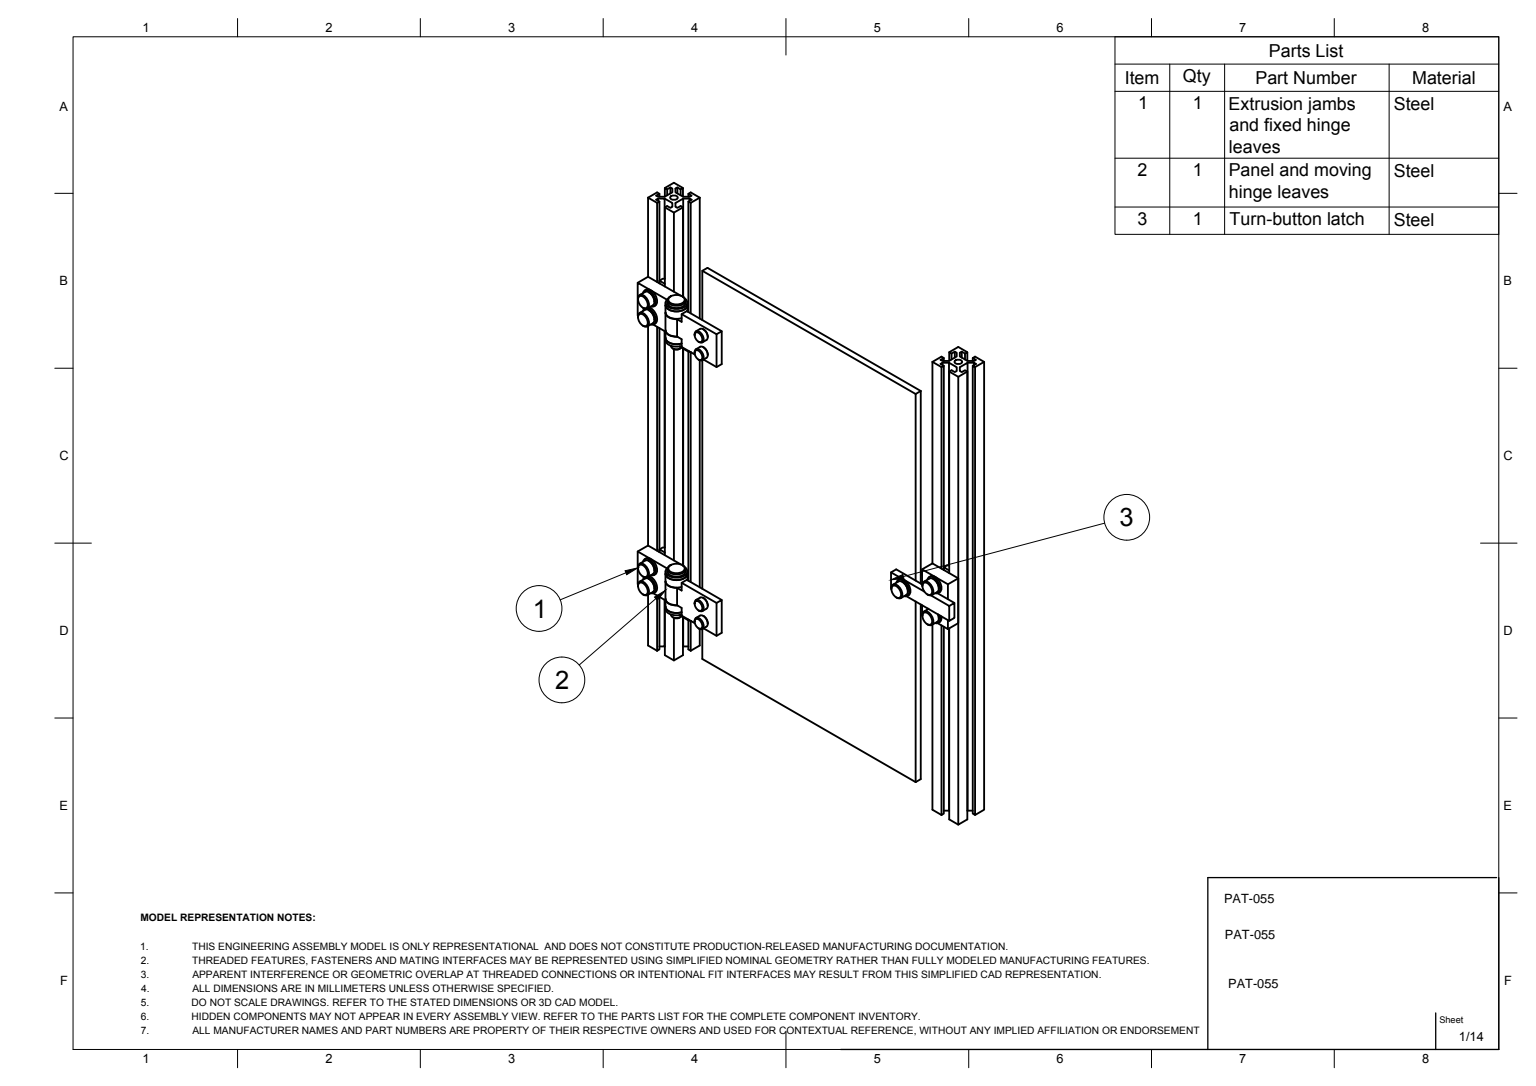
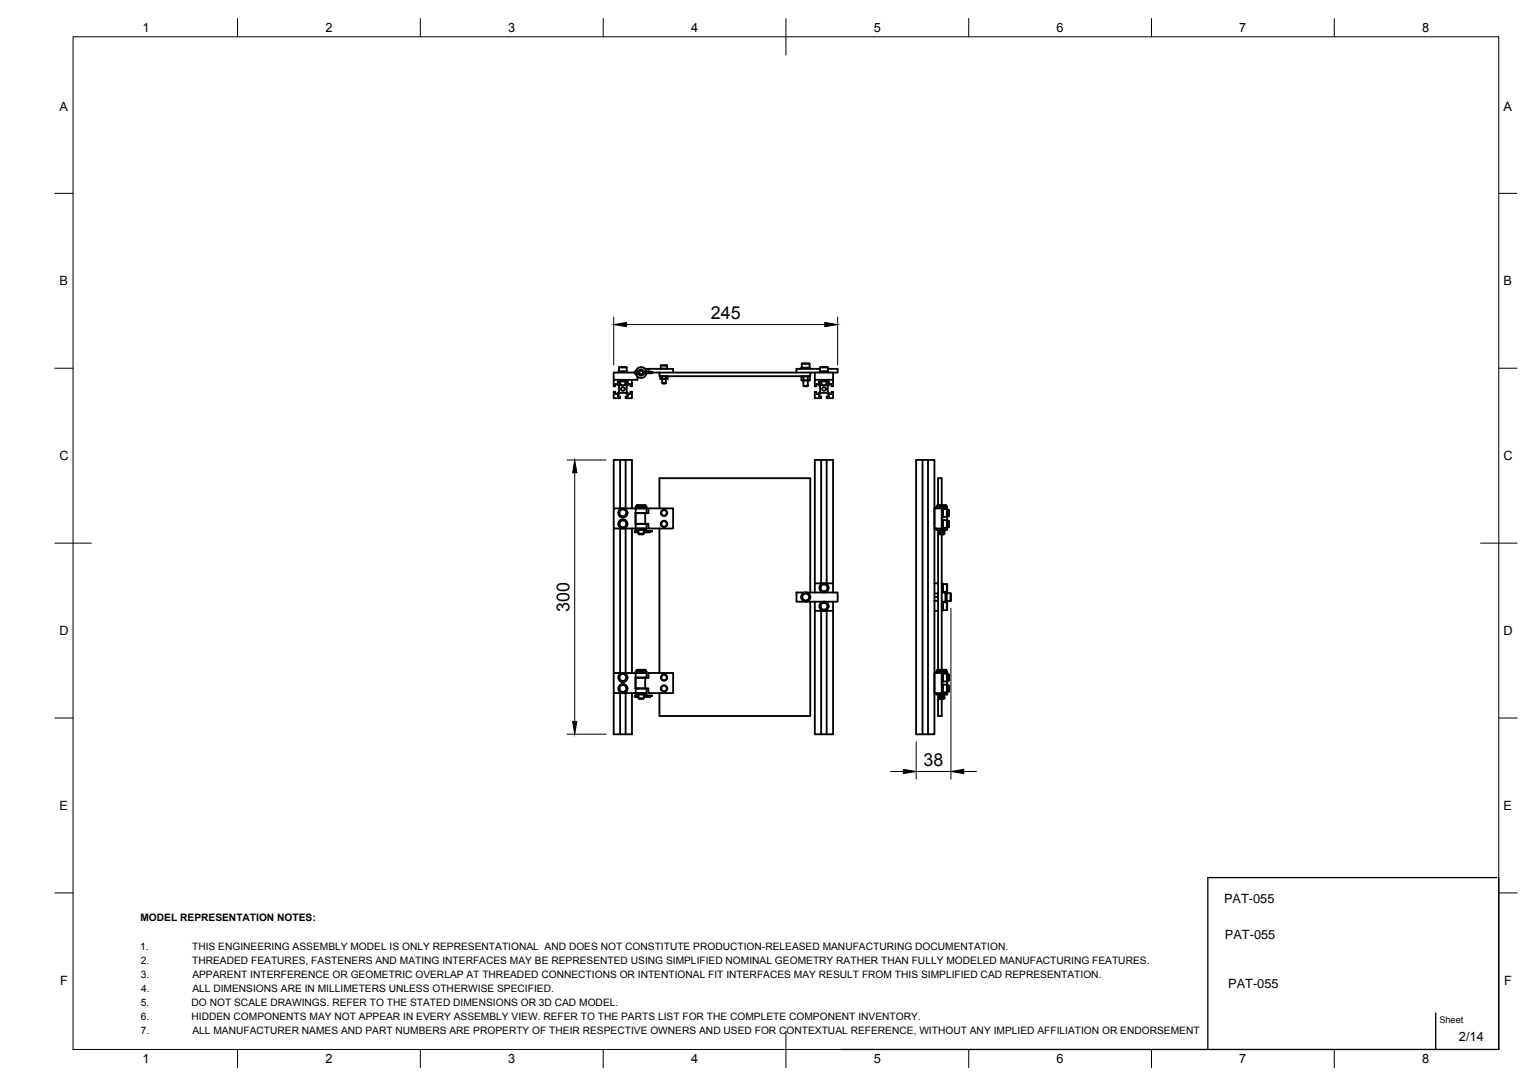
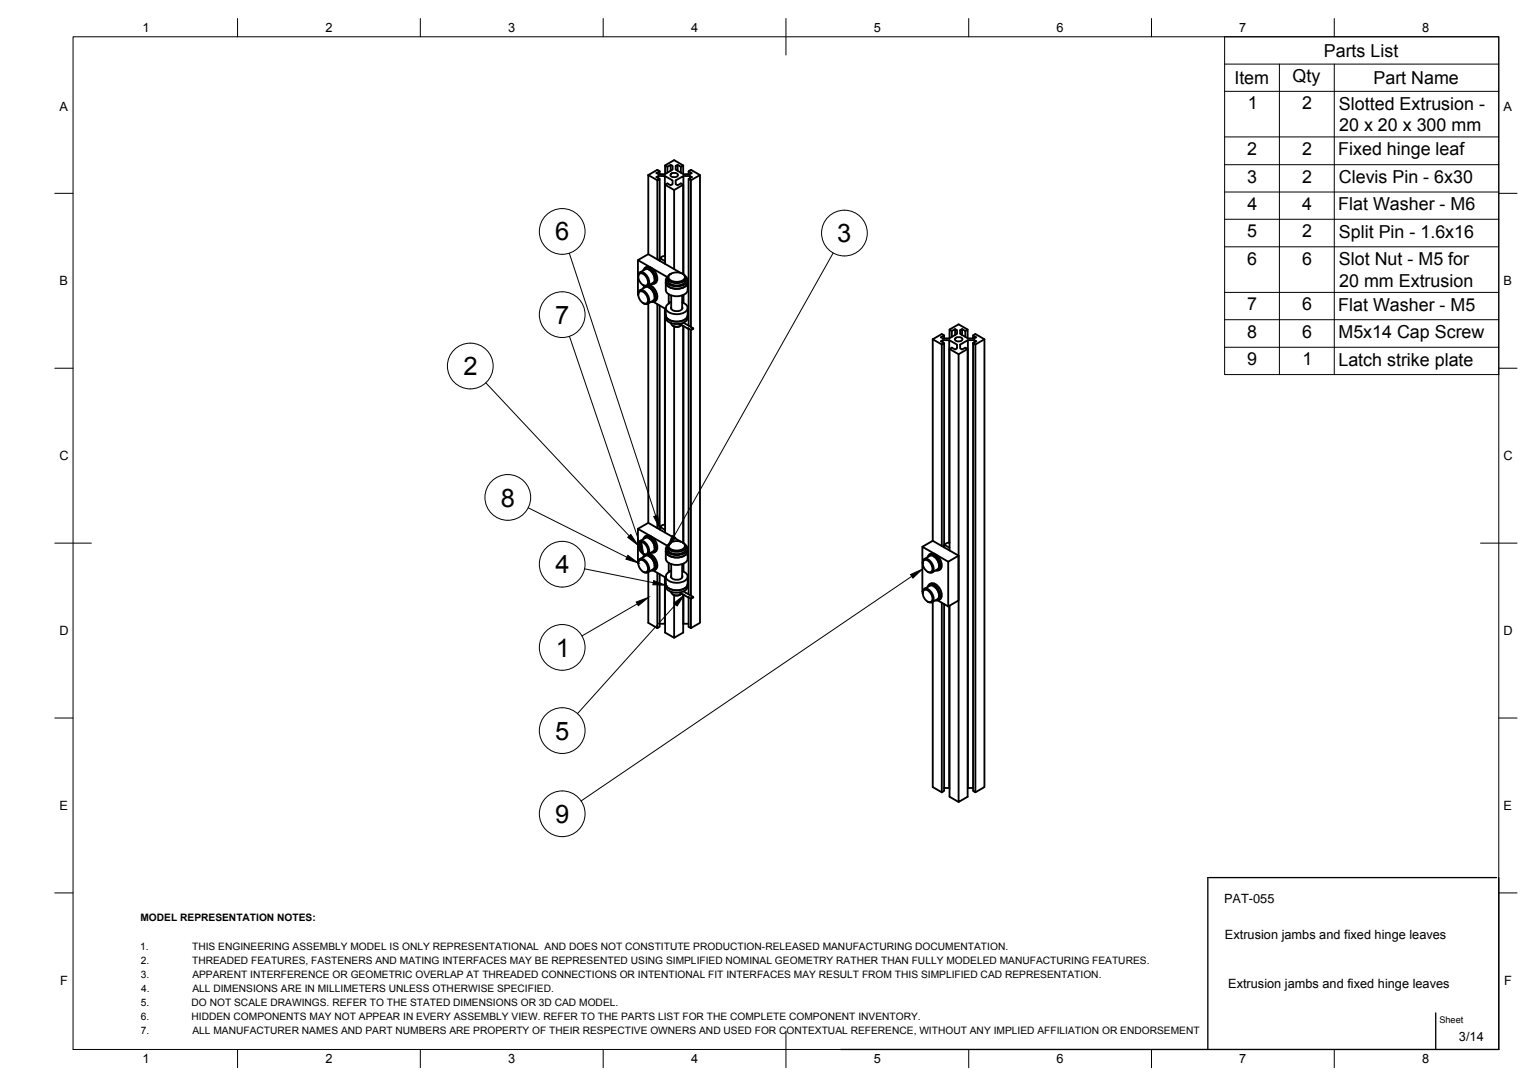
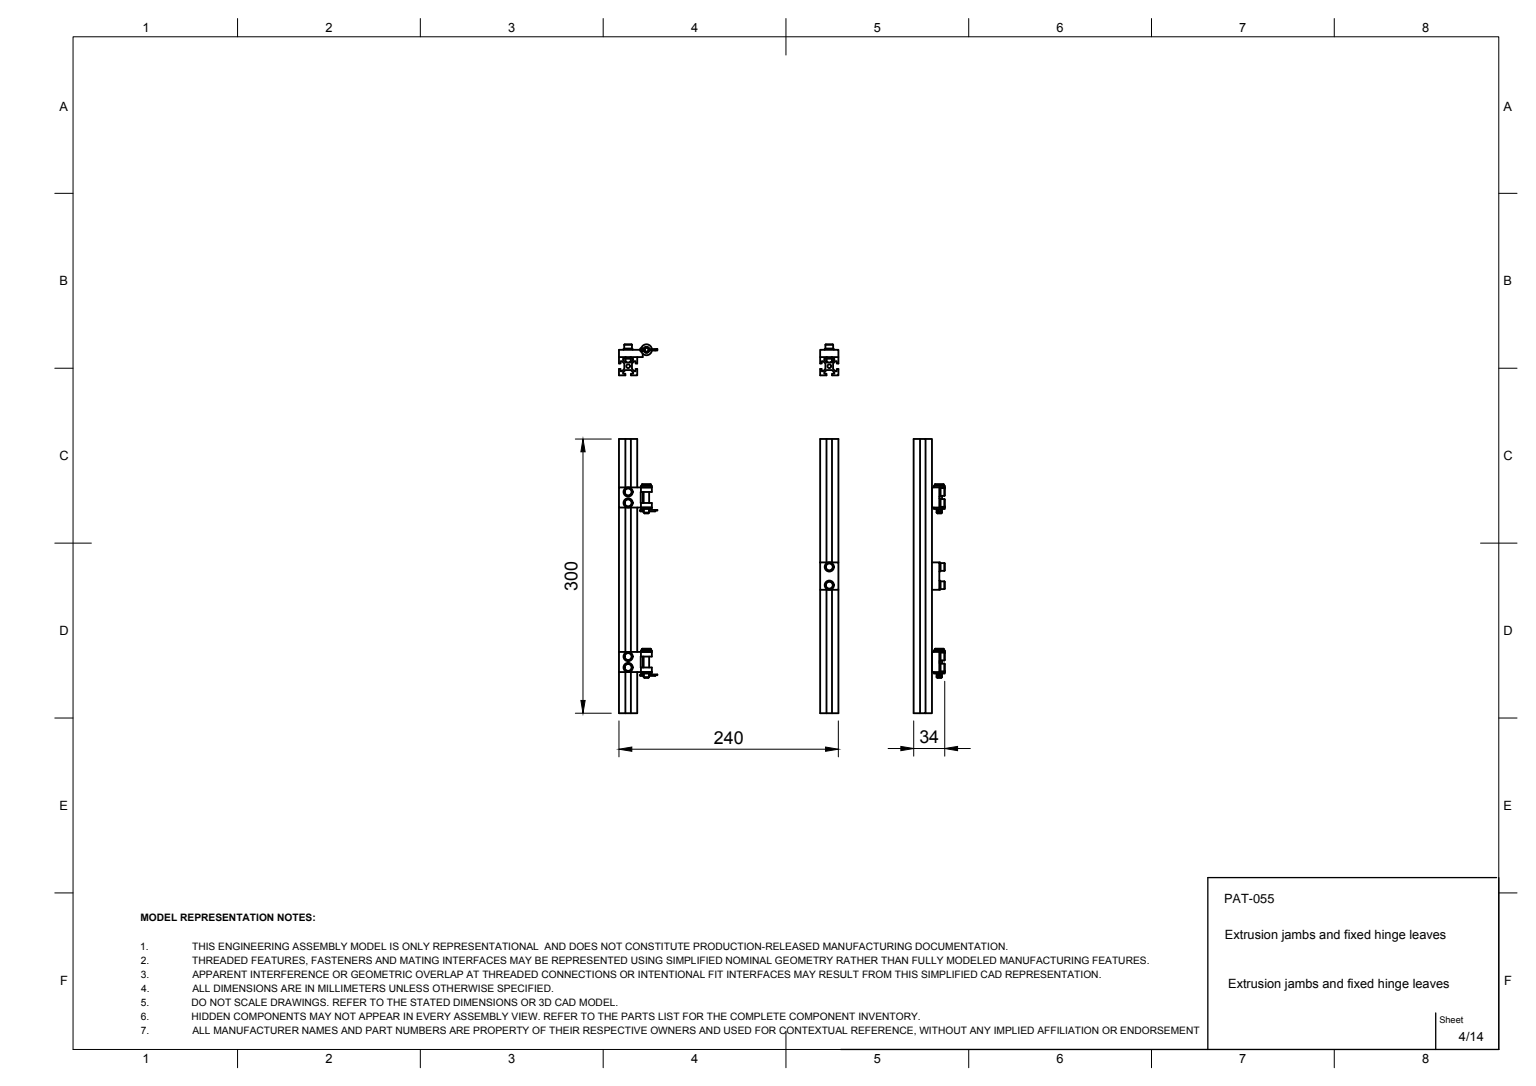
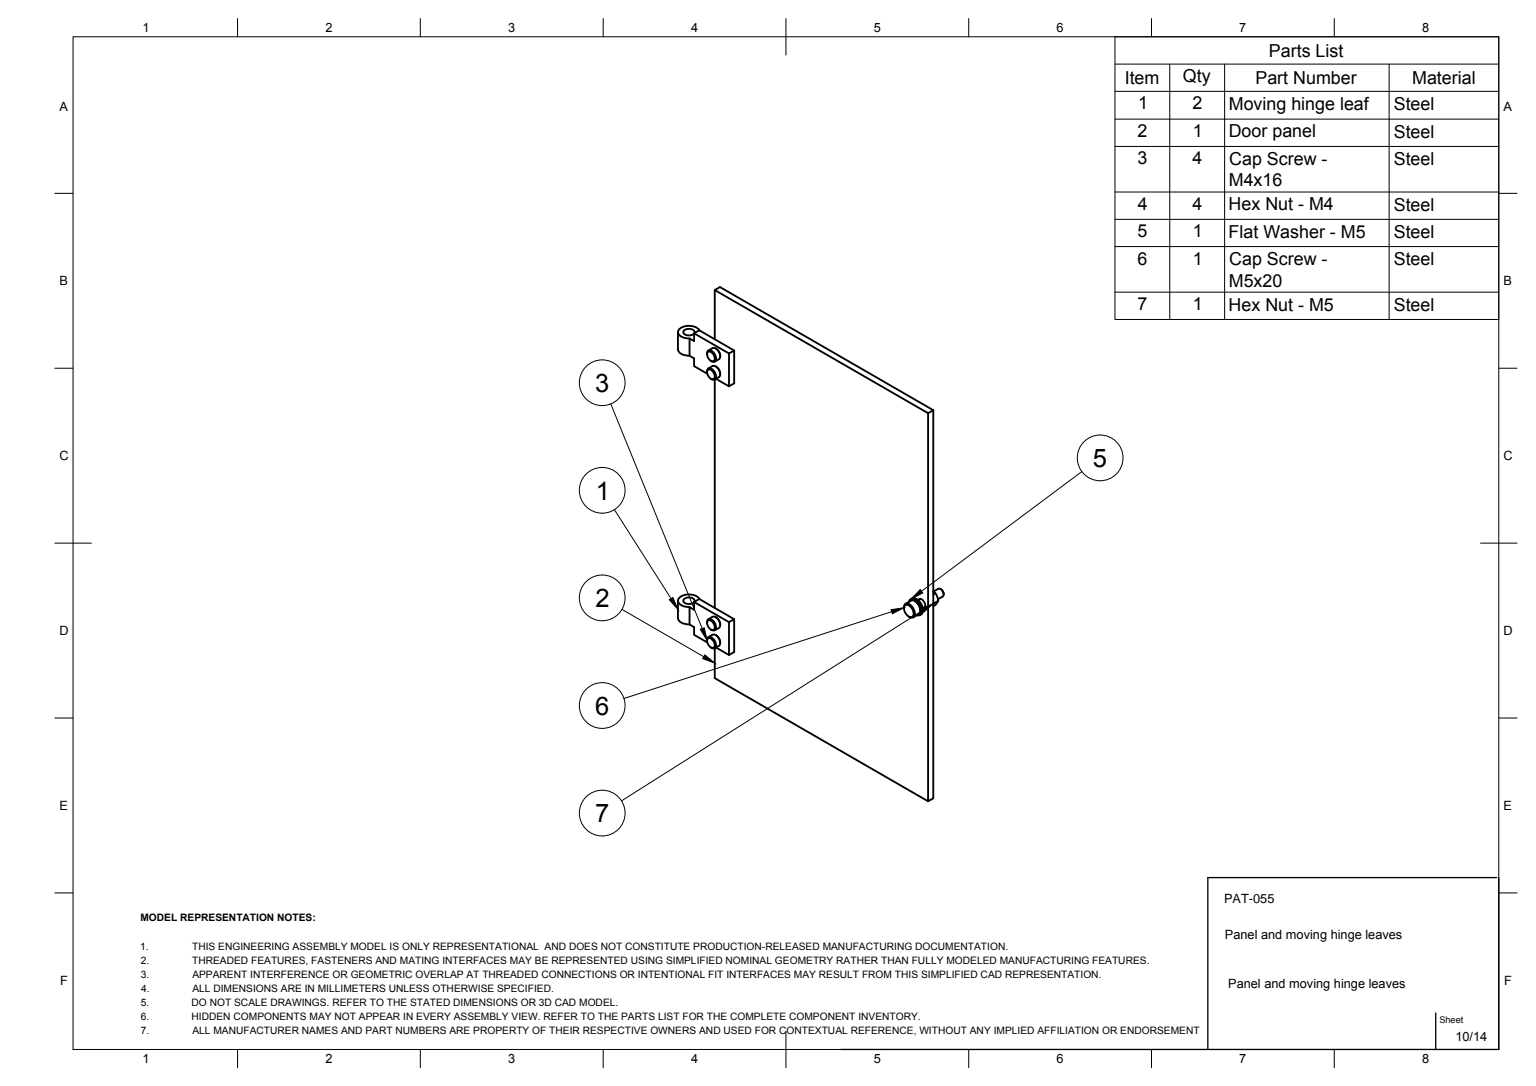
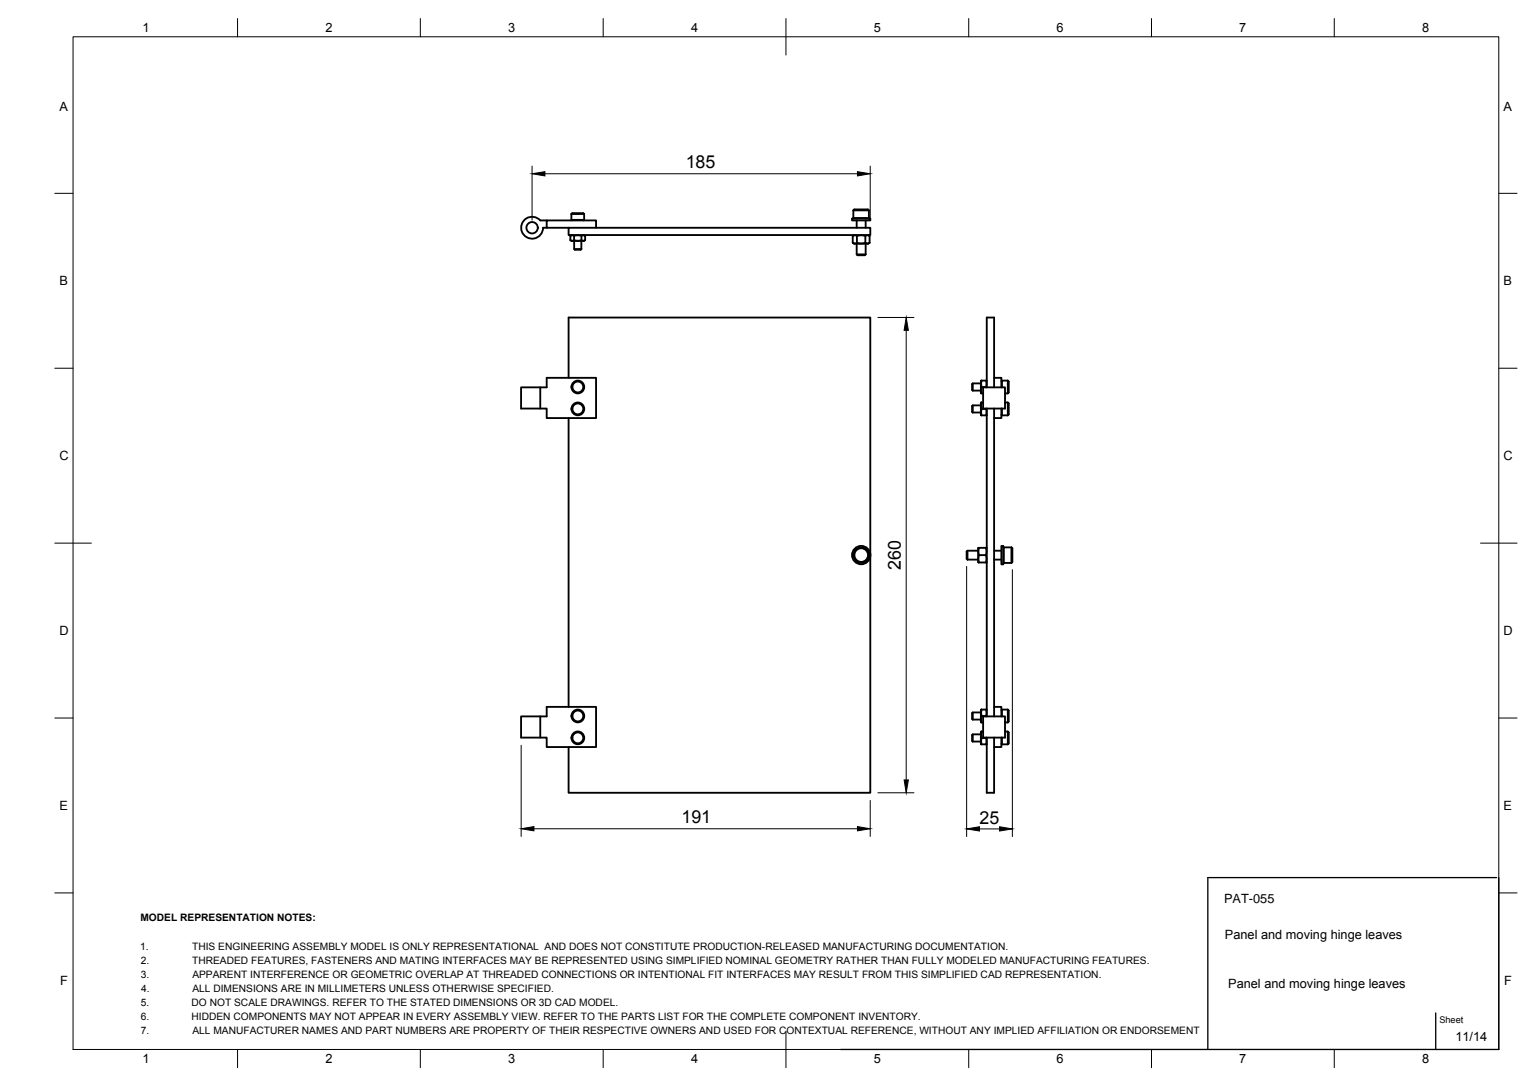
ISO-10303-21;
HEADER;
/* Generated by software containing ST-Developer
 * from STEP Tools, Inc. (www.steptools.com) 
 */

FILE_DESCRIPTION(
/* description */ ('Hinged panel with latch'),
/* implementation_level */ '2;1');

FILE_NAME(
/* name */ 'PAT-055',
/* time_stamp */ '2026-10-27T20:36:01-07:00',
/* author */ (''),
/* organization */ (''),
/* preprocessor_version */ 'ST-DEVELOPER v20.2',
/* originating_system */ 'Autodesk Translation Framework v15.17.0.0',
/* authorisation */ '');

FILE_SCHEMA (('AUTOMOTIVE_DESIGN { 1 0 10303 214 3 1 1 }'));
ENDSEC;

DATA;
#10=MECHANICAL_DESIGN_GEOMETRIC_PRESENTATION_REPRESENTATION('',(#296,#297,
#298,#299,#300,#301,#302,#303,#304,#305,#306,#307,#308,#309,#310,#311),
#6743);
#11=ITEM_DEFINED_TRANSFORMATION($,$,#4059,#4262);
#12=ITEM_DEFINED_TRANSFORMATION($,$,#3996,#4263);
#13=ITEM_DEFINED_TRANSFORMATION($,$,#4009,#4264);
#14=ITEM_DEFINED_TRANSFORMATION($,$,#4009,#4265);
#15=ITEM_DEFINED_TRANSFORMATION($,$,#4059,#4266);
#16=ITEM_DEFINED_TRANSFORMATION($,$,#4088,#4267);
#17=ITEM_DEFINED_TRANSFORMATION($,$,#4103,#4268);
#18=ITEM_DEFINED_TRANSFORMATION($,$,#4103,#4269);
#19=ITEM_DEFINED_TRANSFORMATION($,$,#4112,#4270);
#20=ITEM_DEFINED_TRANSFORMATION($,$,#4123,#4271);
#21=ITEM_DEFINED_TRANSFORMATION($,$,#4251,#4272);
#22=ITEM_DEFINED_TRANSFORMATION($,$,#4140,#4273);
#23=ITEM_DEFINED_TRANSFORMATION($,$,#4123,#4274);
#24=ITEM_DEFINED_TRANSFORMATION($,$,#4251,#4275);
#25=ITEM_DEFINED_TRANSFORMATION($,$,#4140,#4276);
#26=ITEM_DEFINED_TRANSFORMATION($,$,#4088,#4277);
#27=ITEM_DEFINED_TRANSFORMATION($,$,#4103,#4278);
#28=ITEM_DEFINED_TRANSFORMATION($,$,#4103,#4279);
#29=ITEM_DEFINED_TRANSFORMATION($,$,#4112,#4280);
#30=ITEM_DEFINED_TRANSFORMATION($,$,#4123,#4281);
#31=ITEM_DEFINED_TRANSFORMATION($,$,#4251,#4282);
#32=ITEM_DEFINED_TRANSFORMATION($,$,#4140,#4283);
#33=ITEM_DEFINED_TRANSFORMATION($,$,#4123,#4284);
#34=ITEM_DEFINED_TRANSFORMATION($,$,#4251,#4285);
#35=ITEM_DEFINED_TRANSFORMATION($,$,#4140,#4286);
#36=ITEM_DEFINED_TRANSFORMATION($,$,#4123,#4287);
#37=ITEM_DEFINED_TRANSFORMATION($,$,#4251,#4288);
#38=ITEM_DEFINED_TRANSFORMATION($,$,#4140,#4289);
#39=ITEM_DEFINED_TRANSFORMATION($,$,#4123,#4290);
#40=ITEM_DEFINED_TRANSFORMATION($,$,#4251,#4291);
#41=ITEM_DEFINED_TRANSFORMATION($,$,#4140,#4292);
#42=ITEM_DEFINED_TRANSFORMATION($,$,#4187,#4335);
#43=ITEM_DEFINED_TRANSFORMATION($,$,#4165,#4336);
#44=ITEM_DEFINED_TRANSFORMATION($,$,#4187,#4337);
#45=ITEM_DEFINED_TRANSFORMATION($,$,#4209,#4338);
#46=ITEM_DEFINED_TRANSFORMATION($,$,#4235,#4339);
#47=ITEM_DEFINED_TRANSFORMATION($,$,#4209,#4340);
#48=ITEM_DEFINED_TRANSFORMATION($,$,#4235,#4341);
#49=ITEM_DEFINED_TRANSFORMATION($,$,#4209,#4342);
#50=ITEM_DEFINED_TRANSFORMATION($,$,#4235,#4343);
#51=ITEM_DEFINED_TRANSFORMATION($,$,#4209,#4344);
#52=ITEM_DEFINED_TRANSFORMATION($,$,#4235,#4345);
#53=ITEM_DEFINED_TRANSFORMATION($,$,#4251,#4346);
#54=ITEM_DEFINED_TRANSFORMATION($,$,#4293,#4347);
#55=ITEM_DEFINED_TRANSFORMATION($,$,#4319,#4348);
#56=ITEM_DEFINED_TRANSFORMATION($,$,#4350,#4360);
#57=ITEM_DEFINED_TRANSFORMATION($,$,#3995,#4361);
#58=ITEM_DEFINED_TRANSFORMATION($,$,#4164,#4362);
#59=ITEM_DEFINED_TRANSFORMATION($,$,#4349,#4363);
#60=(
REPRESENTATION_RELATIONSHIP($,$,#6841,#6838)
REPRESENTATION_RELATIONSHIP_WITH_TRANSFORMATION(#11)
SHAPE_REPRESENTATION_RELATIONSHIP()
);
#61=(
REPRESENTATION_RELATIONSHIP($,$,#6839,#6838)
REPRESENTATION_RELATIONSHIP_WITH_TRANSFORMATION(#12)
SHAPE_REPRESENTATION_RELATIONSHIP()
);
#62=(
REPRESENTATION_RELATIONSHIP($,$,#6840,#6838)
REPRESENTATION_RELATIONSHIP_WITH_TRANSFORMATION(#13)
SHAPE_REPRESENTATION_RELATIONSHIP()
);
#63=(
REPRESENTATION_RELATIONSHIP($,$,#6840,#6838)
REPRESENTATION_RELATIONSHIP_WITH_TRANSFORMATION(#14)
SHAPE_REPRESENTATION_RELATIONSHIP()
);
#64=(
REPRESENTATION_RELATIONSHIP($,$,#6841,#6838)
REPRESENTATION_RELATIONSHIP_WITH_TRANSFORMATION(#15)
SHAPE_REPRESENTATION_RELATIONSHIP()
);
#65=(
REPRESENTATION_RELATIONSHIP($,$,#6842,#6838)
REPRESENTATION_RELATIONSHIP_WITH_TRANSFORMATION(#16)
SHAPE_REPRESENTATION_RELATIONSHIP()
);
#66=(
REPRESENTATION_RELATIONSHIP($,$,#6843,#6838)
REPRESENTATION_RELATIONSHIP_WITH_TRANSFORMATION(#17)
SHAPE_REPRESENTATION_RELATIONSHIP()
);
#67=(
REPRESENTATION_RELATIONSHIP($,$,#6843,#6838)
REPRESENTATION_RELATIONSHIP_WITH_TRANSFORMATION(#18)
SHAPE_REPRESENTATION_RELATIONSHIP()
);
#68=(
REPRESENTATION_RELATIONSHIP($,$,#6844,#6838)
REPRESENTATION_RELATIONSHIP_WITH_TRANSFORMATION(#19)
SHAPE_REPRESENTATION_RELATIONSHIP()
);
#69=(
REPRESENTATION_RELATIONSHIP($,$,#6845,#6838)
REPRESENTATION_RELATIONSHIP_WITH_TRANSFORMATION(#20)
SHAPE_REPRESENTATION_RELATIONSHIP()
);
#70=(
REPRESENTATION_RELATIONSHIP($,$,#6852,#6838)
REPRESENTATION_RELATIONSHIP_WITH_TRANSFORMATION(#21)
SHAPE_REPRESENTATION_RELATIONSHIP()
);
#71=(
REPRESENTATION_RELATIONSHIP($,$,#6846,#6838)
REPRESENTATION_RELATIONSHIP_WITH_TRANSFORMATION(#22)
SHAPE_REPRESENTATION_RELATIONSHIP()
);
#72=(
REPRESENTATION_RELATIONSHIP($,$,#6845,#6838)
REPRESENTATION_RELATIONSHIP_WITH_TRANSFORMATION(#23)
SHAPE_REPRESENTATION_RELATIONSHIP()
);
#73=(
REPRESENTATION_RELATIONSHIP($,$,#6852,#6838)
REPRESENTATION_RELATIONSHIP_WITH_TRANSFORMATION(#24)
SHAPE_REPRESENTATION_RELATIONSHIP()
);
#74=(
REPRESENTATION_RELATIONSHIP($,$,#6846,#6838)
REPRESENTATION_RELATIONSHIP_WITH_TRANSFORMATION(#25)
SHAPE_REPRESENTATION_RELATIONSHIP()
);
#75=(
REPRESENTATION_RELATIONSHIP($,$,#6842,#6838)
REPRESENTATION_RELATIONSHIP_WITH_TRANSFORMATION(#26)
SHAPE_REPRESENTATION_RELATIONSHIP()
);
#76=(
REPRESENTATION_RELATIONSHIP($,$,#6843,#6838)
REPRESENTATION_RELATIONSHIP_WITH_TRANSFORMATION(#27)
SHAPE_REPRESENTATION_RELATIONSHIP()
);
#77=(
REPRESENTATION_RELATIONSHIP($,$,#6843,#6838)
REPRESENTATION_RELATIONSHIP_WITH_TRANSFORMATION(#28)
SHAPE_REPRESENTATION_RELATIONSHIP()
);
#78=(
REPRESENTATION_RELATIONSHIP($,$,#6844,#6838)
REPRESENTATION_RELATIONSHIP_WITH_TRANSFORMATION(#29)
SHAPE_REPRESENTATION_RELATIONSHIP()
);
#79=(
REPRESENTATION_RELATIONSHIP($,$,#6845,#6838)
REPRESENTATION_RELATIONSHIP_WITH_TRANSFORMATION(#30)
SHAPE_REPRESENTATION_RELATIONSHIP()
);
#80=(
REPRESENTATION_RELATIONSHIP($,$,#6852,#6838)
REPRESENTATION_RELATIONSHIP_WITH_TRANSFORMATION(#31)
SHAPE_REPRESENTATION_RELATIONSHIP()
);
#81=(
REPRESENTATION_RELATIONSHIP($,$,#6846,#6838)
REPRESENTATION_RELATIONSHIP_WITH_TRANSFORMATION(#32)
SHAPE_REPRESENTATION_RELATIONSHIP()
);
#82=(
REPRESENTATION_RELATIONSHIP($,$,#6845,#6838)
REPRESENTATION_RELATIONSHIP_WITH_TRANSFORMATION(#33)
SHAPE_REPRESENTATION_RELATIONSHIP()
);
#83=(
REPRESENTATION_RELATIONSHIP($,$,#6852,#6838)
REPRESENTATION_RELATIONSHIP_WITH_TRANSFORMATION(#34)
SHAPE_REPRESENTATION_RELATIONSHIP()
);
#84=(
REPRESENTATION_RELATIONSHIP($,$,#6846,#6838)
REPRESENTATION_RELATIONSHIP_WITH_TRANSFORMATION(#35)
SHAPE_REPRESENTATION_RELATIONSHIP()
);
#85=(
REPRESENTATION_RELATIONSHIP($,$,#6845,#6838)
REPRESENTATION_RELATIONSHIP_WITH_TRANSFORMATION(#36)
SHAPE_REPRESENTATION_RELATIONSHIP()
);
#86=(
REPRESENTATION_RELATIONSHIP($,$,#6852,#6838)
REPRESENTATION_RELATIONSHIP_WITH_TRANSFORMATION(#37)
SHAPE_REPRESENTATION_RELATIONSHIP()
);
#87=(
REPRESENTATION_RELATIONSHIP($,$,#6846,#6838)
REPRESENTATION_RELATIONSHIP_WITH_TRANSFORMATION(#38)
SHAPE_REPRESENTATION_RELATIONSHIP()
);
#88=(
REPRESENTATION_RELATIONSHIP($,$,#6845,#6838)
REPRESENTATION_RELATIONSHIP_WITH_TRANSFORMATION(#39)
SHAPE_REPRESENTATION_RELATIONSHIP()
);
#89=(
REPRESENTATION_RELATIONSHIP($,$,#6852,#6838)
REPRESENTATION_RELATIONSHIP_WITH_TRANSFORMATION(#40)
SHAPE_REPRESENTATION_RELATIONSHIP()
);
#90=(
REPRESENTATION_RELATIONSHIP($,$,#6846,#6838)
REPRESENTATION_RELATIONSHIP_WITH_TRANSFORMATION(#41)
SHAPE_REPRESENTATION_RELATIONSHIP()
);
#91=(
REPRESENTATION_RELATIONSHIP($,$,#6849,#6847)
REPRESENTATION_RELATIONSHIP_WITH_TRANSFORMATION(#42)
SHAPE_REPRESENTATION_RELATIONSHIP()
);
#92=(
REPRESENTATION_RELATIONSHIP($,$,#6848,#6847)
REPRESENTATION_RELATIONSHIP_WITH_TRANSFORMATION(#43)
SHAPE_REPRESENTATION_RELATIONSHIP()
);
#93=(
REPRESENTATION_RELATIONSHIP($,$,#6849,#6847)
REPRESENTATION_RELATIONSHIP_WITH_TRANSFORMATION(#44)
SHAPE_REPRESENTATION_RELATIONSHIP()
);
#94=(
REPRESENTATION_RELATIONSHIP($,$,#6850,#6847)
REPRESENTATION_RELATIONSHIP_WITH_TRANSFORMATION(#45)
SHAPE_REPRESENTATION_RELATIONSHIP()
);
#95=(
REPRESENTATION_RELATIONSHIP($,$,#6851,#6847)
REPRESENTATION_RELATIONSHIP_WITH_TRANSFORMATION(#46)
SHAPE_REPRESENTATION_RELATIONSHIP()
);
#96=(
REPRESENTATION_RELATIONSHIP($,$,#6850,#6847)
REPRESENTATION_RELATIONSHIP_WITH_TRANSFORMATION(#47)
SHAPE_REPRESENTATION_RELATIONSHIP()
);
#97=(
REPRESENTATION_RELATIONSHIP($,$,#6851,#6847)
REPRESENTATION_RELATIONSHIP_WITH_TRANSFORMATION(#48)
SHAPE_REPRESENTATION_RELATIONSHIP()
);
#98=(
REPRESENTATION_RELATIONSHIP($,$,#6850,#6847)
REPRESENTATION_RELATIONSHIP_WITH_TRANSFORMATION(#49)
SHAPE_REPRESENTATION_RELATIONSHIP()
);
#99=(
REPRESENTATION_RELATIONSHIP($,$,#6851,#6847)
REPRESENTATION_RELATIONSHIP_WITH_TRANSFORMATION(#50)
SHAPE_REPRESENTATION_RELATIONSHIP()
);
#100=(
REPRESENTATION_RELATIONSHIP($,$,#6850,#6847)
REPRESENTATION_RELATIONSHIP_WITH_TRANSFORMATION(#51)
SHAPE_REPRESENTATION_RELATIONSHIP()
);
#101=(
REPRESENTATION_RELATIONSHIP($,$,#6851,#6847)
REPRESENTATION_RELATIONSHIP_WITH_TRANSFORMATION(#52)
SHAPE_REPRESENTATION_RELATIONSHIP()
);
#102=(
REPRESENTATION_RELATIONSHIP($,$,#6852,#6847)
REPRESENTATION_RELATIONSHIP_WITH_TRANSFORMATION(#53)
SHAPE_REPRESENTATION_RELATIONSHIP()
);
#103=(
REPRESENTATION_RELATIONSHIP($,$,#6853,#6847)
REPRESENTATION_RELATIONSHIP_WITH_TRANSFORMATION(#54)
SHAPE_REPRESENTATION_RELATIONSHIP()
);
#104=(
REPRESENTATION_RELATIONSHIP($,$,#6854,#6847)
REPRESENTATION_RELATIONSHIP_WITH_TRANSFORMATION(#55)
SHAPE_REPRESENTATION_RELATIONSHIP()
);
#105=(
REPRESENTATION_RELATIONSHIP($,$,#6856,#6855)
REPRESENTATION_RELATIONSHIP_WITH_TRANSFORMATION(#56)
SHAPE_REPRESENTATION_RELATIONSHIP()
);
#106=(
REPRESENTATION_RELATIONSHIP($,$,#6838,#6837)
REPRESENTATION_RELATIONSHIP_WITH_TRANSFORMATION(#57)
SHAPE_REPRESENTATION_RELATIONSHIP()
);
#107=(
REPRESENTATION_RELATIONSHIP($,$,#6847,#6837)
REPRESENTATION_RELATIONSHIP_WITH_TRANSFORMATION(#58)
SHAPE_REPRESENTATION_RELATIONSHIP()
);
#108=(
REPRESENTATION_RELATIONSHIP($,$,#6855,#6837)
REPRESENTATION_RELATIONSHIP_WITH_TRANSFORMATION(#59)
SHAPE_REPRESENTATION_RELATIONSHIP()
);
#109=CONTEXT_DEPENDENT_SHAPE_REPRESENTATION(#60,#6784);
#110=CONTEXT_DEPENDENT_SHAPE_REPRESENTATION(#61,#6785);
#111=CONTEXT_DEPENDENT_SHAPE_REPRESENTATION(#62,#6786);
#112=CONTEXT_DEPENDENT_SHAPE_REPRESENTATION(#63,#6787);
#113=CONTEXT_DEPENDENT_SHAPE_REPRESENTATION(#64,#6788);
#114=CONTEXT_DEPENDENT_SHAPE_REPRESENTATION(#65,#6789);
#115=CONTEXT_DEPENDENT_SHAPE_REPRESENTATION(#66,#6790);
#116=CONTEXT_DEPENDENT_SHAPE_REPRESENTATION(#67,#6791);
#117=CONTEXT_DEPENDENT_SHAPE_REPRESENTATION(#68,#6792);
#118=CONTEXT_DEPENDENT_SHAPE_REPRESENTATION(#69,#6793);
#119=CONTEXT_DEPENDENT_SHAPE_REPRESENTATION(#70,#6794);
#120=CONTEXT_DEPENDENT_SHAPE_REPRESENTATION(#71,#6795);
#121=CONTEXT_DEPENDENT_SHAPE_REPRESENTATION(#72,#6796);
#122=CONTEXT_DEPENDENT_SHAPE_REPRESENTATION(#73,#6797);
#123=CONTEXT_DEPENDENT_SHAPE_REPRESENTATION(#74,#6798);
#124=CONTEXT_DEPENDENT_SHAPE_REPRESENTATION(#75,#6799);
#125=CONTEXT_DEPENDENT_SHAPE_REPRESENTATION(#76,#6800);
#126=CONTEXT_DEPENDENT_SHAPE_REPRESENTATION(#77,#6801);
#127=CONTEXT_DEPENDENT_SHAPE_REPRESENTATION(#78,#6802);
#128=CONTEXT_DEPENDENT_SHAPE_REPRESENTATION(#79,#6803);
#129=CONTEXT_DEPENDENT_SHAPE_REPRESENTATION(#80,#6804);
#130=CONTEXT_DEPENDENT_SHAPE_REPRESENTATION(#81,#6805);
#131=CONTEXT_DEPENDENT_SHAPE_REPRESENTATION(#82,#6806);
#132=CONTEXT_DEPENDENT_SHAPE_REPRESENTATION(#83,#6807);
#133=CONTEXT_DEPENDENT_SHAPE_REPRESENTATION(#84,#6808);
#134=CONTEXT_DEPENDENT_SHAPE_REPRESENTATION(#85,#6809);
#135=CONTEXT_DEPENDENT_SHAPE_REPRESENTATION(#86,#6810);
#136=CONTEXT_DEPENDENT_SHAPE_REPRESENTATION(#87,#6811);
#137=CONTEXT_DEPENDENT_SHAPE_REPRESENTATION(#88,#6812);
#138=CONTEXT_DEPENDENT_SHAPE_REPRESENTATION(#89,#6813);
#139=CONTEXT_DEPENDENT_SHAPE_REPRESENTATION(#90,#6814);
#140=CONTEXT_DEPENDENT_SHAPE_REPRESENTATION(#91,#6817);
#141=CONTEXT_DEPENDENT_SHAPE_REPRESENTATION(#92,#6818);
#142=CONTEXT_DEPENDENT_SHAPE_REPRESENTATION(#93,#6819);
#143=CONTEXT_DEPENDENT_SHAPE_REPRESENTATION(#94,#6820);
#144=CONTEXT_DEPENDENT_SHAPE_REPRESENTATION(#95,#6821);
#145=CONTEXT_DEPENDENT_SHAPE_REPRESENTATION(#96,#6822);
#146=CONTEXT_DEPENDENT_SHAPE_REPRESENTATION(#97,#6823);
#147=CONTEXT_DEPENDENT_SHAPE_REPRESENTATION(#98,#6824);
#148=CONTEXT_DEPENDENT_SHAPE_REPRESENTATION(#99,#6825);
#149=CONTEXT_DEPENDENT_SHAPE_REPRESENTATION(#100,#6826);
#150=CONTEXT_DEPENDENT_SHAPE_REPRESENTATION(#101,#6827);
#151=CONTEXT_DEPENDENT_SHAPE_REPRESENTATION(#102,#6828);
#152=CONTEXT_DEPENDENT_SHAPE_REPRESENTATION(#103,#6829);
#153=CONTEXT_DEPENDENT_SHAPE_REPRESENTATION(#104,#6830);
#154=CONTEXT_DEPENDENT_SHAPE_REPRESENTATION(#105,#6833);
#155=CONTEXT_DEPENDENT_SHAPE_REPRESENTATION(#106,#6834);
#156=CONTEXT_DEPENDENT_SHAPE_REPRESENTATION(#107,#6835);
#157=CONTEXT_DEPENDENT_SHAPE_REPRESENTATION(#108,#6836);
#158=NEXT_ASSEMBLY_USAGE_OCCURRENCE('Fixed hinge leaf:1',
'Fixed hinge leaf:1','Fixed hinge leaf:1',#6859,#6862,
'Fixed hinge leaf:1');
#159=NEXT_ASSEMBLY_USAGE_OCCURRENCE('Latch strike plate:1',
'Latch strike plate:1','Latch strike plate:1',#6859,#6860,
'Latch strike plate:1');
#160=NEXT_ASSEMBLY_USAGE_OCCURRENCE(
'Slotted Extrusion - 20 x 20 x 300 mm:2',
'Slotted Extrusion - 20 x 20 x 300 mm:2',
'Slotted Extrusion - 20 x 20 x 300 mm:2',#6859,#6861,
'Slotted Extrusion - 20 x 20 x 300 mm:2');
#161=NEXT_ASSEMBLY_USAGE_OCCURRENCE(
'Slotted Extrusion - 20 x 20 x 300 mm:3',
'Slotted Extrusion - 20 x 20 x 300 mm:3',
'Slotted Extrusion - 20 x 20 x 300 mm:3',#6859,#6861,
'Slotted Extrusion - 20 x 20 x 300 mm:3');
#162=NEXT_ASSEMBLY_USAGE_OCCURRENCE('Fixed hinge leaf:2',
'Fixed hinge leaf:2','Fixed hinge leaf:2',#6859,#6862,
'Fixed hinge leaf:2');
#163=NEXT_ASSEMBLY_USAGE_OCCURRENCE('Clevis Pin - 6x30:2',
'Clevis Pin - 6x30:2','Clevis Pin - 6x30:2',#6859,#6863,
'Clevis Pin - 6x30:2');
#164=NEXT_ASSEMBLY_USAGE_OCCURRENCE('Flat Washer - M6:2',
'Flat Washer - M6:2','Flat Washer - M6:2',#6859,#6864,
'Flat Washer - M6:2');
#165=NEXT_ASSEMBLY_USAGE_OCCURRENCE('Flat Washer - M6:3',
'Flat Washer - M6:3','Flat Washer - M6:3',#6859,#6864,
'Flat Washer - M6:3');
#166=NEXT_ASSEMBLY_USAGE_OCCURRENCE('Split Pin - 1.6x16:2',
'Split Pin - 1.6x16:2','Split Pin - 1.6x16:2',#6859,#6865,
'Split Pin - 1.6x16:2');
#167=NEXT_ASSEMBLY_USAGE_OCCURRENCE(
'Slot Nut - M5 for 20 mm Extrusion:2',
'Slot Nut - M5 for 20 mm Extrusion:2',
'Slot Nut - M5 for 20 mm Extrusion:2',#6859,#6866,
'Slot Nut - M5 for 20 mm Extrusion:2');
#168=NEXT_ASSEMBLY_USAGE_OCCURRENCE('Flat Washer - M5:2',
'Flat Washer - M5:2','Flat Washer - M5:2',#6859,#6873,
'Flat Washer - M5:2');
#169=NEXT_ASSEMBLY_USAGE_OCCURRENCE('M5x14 Cap Screw:2',
'M5x14 Cap Screw:2','M5x14 Cap Screw:2',#6859,#6867,'M5x14 Cap Screw:2');
#170=NEXT_ASSEMBLY_USAGE_OCCURRENCE(
'Slot Nut - M5 for 20 mm Extrusion:3',
'Slot Nut - M5 for 20 mm Extrusion:3',
'Slot Nut - M5 for 20 mm Extrusion:3',#6859,#6866,
'Slot Nut - M5 for 20 mm Extrusion:3');
#171=NEXT_ASSEMBLY_USAGE_OCCURRENCE('Flat Washer - M5:3',
'Flat Washer - M5:3','Flat Washer - M5:3',#6859,#6873,
'Flat Washer - M5:3');
#172=NEXT_ASSEMBLY_USAGE_OCCURRENCE('M5x14 Cap Screw:3',
'M5x14 Cap Screw:3','M5x14 Cap Screw:3',#6859,#6867,'M5x14 Cap Screw:3');
#173=NEXT_ASSEMBLY_USAGE_OCCURRENCE('Clevis Pin - 6x30:3',
'Clevis Pin - 6x30:3','Clevis Pin - 6x30:3',#6859,#6863,
'Clevis Pin - 6x30:3');
#174=NEXT_ASSEMBLY_USAGE_OCCURRENCE('Flat Washer - M6:4',
'Flat Washer - M6:4','Flat Washer - M6:4',#6859,#6864,
'Flat Washer - M6:4');
#175=NEXT_ASSEMBLY_USAGE_OCCURRENCE('Flat Washer - M6:5',
'Flat Washer - M6:5','Flat Washer - M6:5',#6859,#6864,
'Flat Washer - M6:5');
#176=NEXT_ASSEMBLY_USAGE_OCCURRENCE('Split Pin - 1.6x16:3',
'Split Pin - 1.6x16:3','Split Pin - 1.6x16:3',#6859,#6865,
'Split Pin - 1.6x16:3');
#177=NEXT_ASSEMBLY_USAGE_OCCURRENCE(
'Slot Nut - M5 for 20 mm Extrusion:4',
'Slot Nut - M5 for 20 mm Extrusion:4',
'Slot Nut - M5 for 20 mm Extrusion:4',#6859,#6866,
'Slot Nut - M5 for 20 mm Extrusion:4');
#178=NEXT_ASSEMBLY_USAGE_OCCURRENCE('Flat Washer - M5:4',
'Flat Washer - M5:4','Flat Washer - M5:4',#6859,#6873,
'Flat Washer - M5:4');
#179=NEXT_ASSEMBLY_USAGE_OCCURRENCE('M5x14 Cap Screw:4',
'M5x14 Cap Screw:4','M5x14 Cap Screw:4',#6859,#6867,'M5x14 Cap Screw:4');
#180=NEXT_ASSEMBLY_USAGE_OCCURRENCE(
'Slot Nut - M5 for 20 mm Extrusion:5',
'Slot Nut - M5 for 20 mm Extrusion:5',
'Slot Nut - M5 for 20 mm Extrusion:5',#6859,#6866,
'Slot Nut - M5 for 20 mm Extrusion:5');
#181=NEXT_ASSEMBLY_USAGE_OCCURRENCE('Flat Washer - M5:5',
'Flat Washer - M5:5','Flat Washer - M5:5',#6859,#6873,
'Flat Washer - M5:5');
#182=NEXT_ASSEMBLY_USAGE_OCCURRENCE('M5x14 Cap Screw:5',
'M5x14 Cap Screw:5','M5x14 Cap Screw:5',#6859,#6867,'M5x14 Cap Screw:5');
#183=NEXT_ASSEMBLY_USAGE_OCCURRENCE(
'Slot Nut - M5 for 20 mm Extrusion:6',
'Slot Nut - M5 for 20 mm Extrusion:6',
'Slot Nut - M5 for 20 mm Extrusion:6',#6859,#6866,
'Slot Nut - M5 for 20 mm Extrusion:6');
#184=NEXT_ASSEMBLY_USAGE_OCCURRENCE('Flat Washer - M5:6',
'Flat Washer - M5:6','Flat Washer - M5:6',#6859,#6873,
'Flat Washer - M5:6');
#185=NEXT_ASSEMBLY_USAGE_OCCURRENCE('M5x14 Cap Screw:6',
'M5x14 Cap Screw:6','M5x14 Cap Screw:6',#6859,#6867,'M5x14 Cap Screw:6');
#186=NEXT_ASSEMBLY_USAGE_OCCURRENCE(
'Slot Nut - M5 for 20 mm Extrusion:7',
'Slot Nut - M5 for 20 mm Extrusion:7',
'Slot Nut - M5 for 20 mm Extrusion:7',#6859,#6866,
'Slot Nut - M5 for 20 mm Extrusion:7');
#187=NEXT_ASSEMBLY_USAGE_OCCURRENCE('Flat Washer - M5:7',
'Flat Washer - M5:7','Flat Washer - M5:7',#6859,#6873,
'Flat Washer - M5:7');
#188=NEXT_ASSEMBLY_USAGE_OCCURRENCE('M5x14 Cap Screw:7',
'M5x14 Cap Screw:7','M5x14 Cap Screw:7',#6859,#6867,'M5x14 Cap Screw:7');
#189=NEXT_ASSEMBLY_USAGE_OCCURRENCE('Moving hinge leaf:1',
'Moving hinge leaf:1','Moving hinge leaf:1',#6868,#6870,
'Moving hinge leaf:1');
#190=NEXT_ASSEMBLY_USAGE_OCCURRENCE('Door panel:1','Door panel:1',
'Door panel:1',#6868,#6869,'Door panel:1');
#191=NEXT_ASSEMBLY_USAGE_OCCURRENCE('Moving hinge leaf:2',
'Moving hinge leaf:2','Moving hinge leaf:2',#6868,#6870,
'Moving hinge leaf:2');
#192=NEXT_ASSEMBLY_USAGE_OCCURRENCE('Cap Screw - M4x16:2',
'Cap Screw - M4x16:2','Cap Screw - M4x16:2',#6868,#6871,
'Cap Screw - M4x16:2');
#193=NEXT_ASSEMBLY_USAGE_OCCURRENCE('Hex Nut - M4:2','Hex Nut - M4:2',
'Hex Nut - M4:2',#6868,#6872,'Hex Nut - M4:2');
#194=NEXT_ASSEMBLY_USAGE_OCCURRENCE('Cap Screw - M4x16:3',
'Cap Screw - M4x16:3','Cap Screw - M4x16:3',#6868,#6871,
'Cap Screw - M4x16:3');
#195=NEXT_ASSEMBLY_USAGE_OCCURRENCE('Hex Nut - M4:3','Hex Nut - M4:3',
'Hex Nut - M4:3',#6868,#6872,'Hex Nut - M4:3');
#196=NEXT_ASSEMBLY_USAGE_OCCURRENCE('Cap Screw - M4x16:4',
'Cap Screw - M4x16:4','Cap Screw - M4x16:4',#6868,#6871,
'Cap Screw - M4x16:4');
#197=NEXT_ASSEMBLY_USAGE_OCCURRENCE('Hex Nut - M4:4','Hex Nut - M4:4',
'Hex Nut - M4:4',#6868,#6872,'Hex Nut - M4:4');
#198=NEXT_ASSEMBLY_USAGE_OCCURRENCE('Cap Screw - M4x16:5',
'Cap Screw - M4x16:5','Cap Screw - M4x16:5',#6868,#6871,
'Cap Screw - M4x16:5');
#199=NEXT_ASSEMBLY_USAGE_OCCURRENCE('Hex Nut - M4:5','Hex Nut - M4:5',
'Hex Nut - M4:5',#6868,#6872,'Hex Nut - M4:5');
#200=NEXT_ASSEMBLY_USAGE_OCCURRENCE('Flat Washer - M5:8',
'Flat Washer - M5:8','Flat Washer - M5:8',#6868,#6873,
'Flat Washer - M5:8');
#201=NEXT_ASSEMBLY_USAGE_OCCURRENCE('Cap Screw - M5x20:2',
'Cap Screw - M5x20:2','Cap Screw - M5x20:2',#6868,#6874,
'Cap Screw - M5x20:2');
#202=NEXT_ASSEMBLY_USAGE_OCCURRENCE('Hex Nut - M5:2','Hex Nut - M5:2',
'Hex Nut - M5:2',#6868,#6875,'Hex Nut - M5:2');
#203=NEXT_ASSEMBLY_USAGE_OCCURRENCE('Turn-button latch (1):1',
'Turn-button latch (1):1','Turn-button latch (1):1',#6876,#6877,
'Turn-button latch (1):1');
#204=NEXT_ASSEMBLY_USAGE_OCCURRENCE(
'Extrusion jambs and fixed hinge leaves:1',
'Extrusion jambs and fixed hinge leaves:1',
'Extrusion jambs and fixed hinge leaves:1',#6858,#6859,
'Extrusion jambs and fixed hinge leaves:1');
#205=NEXT_ASSEMBLY_USAGE_OCCURRENCE('Panel and moving hinge leaves:1',
'Panel and moving hinge leaves:1','Panel and moving hinge leaves:1',#6858,
#6868,'Panel and moving hinge leaves:1');
#206=NEXT_ASSEMBLY_USAGE_OCCURRENCE('Turn-button latch:1',
'Turn-button latch:1','Turn-button latch:1',#6858,#6876,
'Turn-button latch:1');
#207=(
BOUNDED_CURVE()
B_SPLINE_CURVE(2,(#6380,#6381,#6382),.UNSPECIFIED.,.F.,.F.)
B_SPLINE_CURVE_WITH_KNOTS((3,3),(0.137956735689167,0.609258407070138),
 .UNSPECIFIED.)
CURVE()
GEOMETRIC_REPRESENTATION_ITEM()
RATIONAL_B_SPLINE_CURVE((1.13260046146793,1.30781436262561,1.13260046146793))
REPRESENTATION_ITEM('')
);
#208=(
BOUNDED_CURVE()
B_SPLINE_CURVE(2,(#6384,#6385,#6386),.UNSPECIFIED.,.F.,.F.)
B_SPLINE_CURVE_WITH_KNOTS((3,3),(0.137956735689167,0.609258407070137),
 .UNSPECIFIED.)
CURVE()
GEOMETRIC_REPRESENTATION_ITEM()
RATIONAL_B_SPLINE_CURVE((1.13260046146793,1.30781436262561,1.13260046146793))
REPRESENTATION_ITEM('')
);
#209=(
BOUNDED_CURVE()
B_SPLINE_CURVE(2,(#6391,#6392,#6393),.UNSPECIFIED.,.F.,.F.)
B_SPLINE_CURVE_WITH_KNOTS((3,3),(0.137956735689167,0.609258407070138),
 .UNSPECIFIED.)
CURVE()
GEOMETRIC_REPRESENTATION_ITEM()
RATIONAL_B_SPLINE_CURVE((1.13260046146793,1.30781436262561,1.13260046146793))
REPRESENTATION_ITEM('')
);
#210=(
BOUNDED_CURVE()
B_SPLINE_CURVE(2,(#6395,#6396,#6397),.UNSPECIFIED.,.F.,.F.)
B_SPLINE_CURVE_WITH_KNOTS((3,3),(0.137956735689167,0.609258407070138),
 .UNSPECIFIED.)
CURVE()
GEOMETRIC_REPRESENTATION_ITEM()
RATIONAL_B_SPLINE_CURVE((1.13260046146793,1.30781436262561,1.13260046146793))
REPRESENTATION_ITEM('')
);
#211=(
BOUNDED_CURVE()
B_SPLINE_CURVE(2,(#6399,#6400,#6401),.UNSPECIFIED.,.F.,.F.)
B_SPLINE_CURVE_WITH_KNOTS((3,3),(0.137956735689167,0.609258407070138),
 .UNSPECIFIED.)
CURVE()
GEOMETRIC_REPRESENTATION_ITEM()
RATIONAL_B_SPLINE_CURVE((1.13260046146793,1.30781436262561,1.13260046146793))
REPRESENTATION_ITEM('')
);
#212=(
BOUNDED_CURVE()
B_SPLINE_CURVE(2,(#6402,#6403,#6404),.UNSPECIFIED.,.F.,.F.)
B_SPLINE_CURVE_WITH_KNOTS((3,3),(0.137956735689167,0.609258407070138),
 .UNSPECIFIED.)
CURVE()
GEOMETRIC_REPRESENTATION_ITEM()
RATIONAL_B_SPLINE_CURVE((1.13260046146793,1.30781436262561,1.13260046146793))
REPRESENTATION_ITEM('')
);
#213=(
BOUNDED_CURVE()
B_SPLINE_CURVE(2,(#6411,#6412,#6413),.UNSPECIFIED.,.F.,.F.)
B_SPLINE_CURVE_WITH_KNOTS((3,3),(0.137956735689167,0.609258407070138),
 .UNSPECIFIED.)
CURVE()
GEOMETRIC_REPRESENTATION_ITEM()
RATIONAL_B_SPLINE_CURVE((1.13260046146793,1.30781436262561,1.13260046146793))
REPRESENTATION_ITEM('')
);
#214=(
BOUNDED_CURVE()
B_SPLINE_CURVE(2,(#6415,#6416,#6417),.UNSPECIFIED.,.F.,.F.)
B_SPLINE_CURVE_WITH_KNOTS((3,3),(0.137956735689167,0.609258407070138),
 .UNSPECIFIED.)
CURVE()
GEOMETRIC_REPRESENTATION_ITEM()
RATIONAL_B_SPLINE_CURVE((1.13260046146793,1.30781436262561,1.13260046146793))
REPRESENTATION_ITEM('')
);
#215=(
BOUNDED_CURVE()
B_SPLINE_CURVE(2,(#6419,#6420,#6421),.UNSPECIFIED.,.F.,.F.)
B_SPLINE_CURVE_WITH_KNOTS((3,3),(0.137956735689167,0.609258407070138),
 .UNSPECIFIED.)
CURVE()
GEOMETRIC_REPRESENTATION_ITEM()
RATIONAL_B_SPLINE_CURVE((1.13260046146793,1.30781436262561,1.13260046146793))
REPRESENTATION_ITEM('')
);
#216=(
BOUNDED_CURVE()
B_SPLINE_CURVE(2,(#6423,#6424,#6425),.UNSPECIFIED.,.F.,.F.)
B_SPLINE_CURVE_WITH_KNOTS((3,3),(0.137956735689167,0.609258407070138),
 .UNSPECIFIED.)
CURVE()
GEOMETRIC_REPRESENTATION_ITEM()
RATIONAL_B_SPLINE_CURVE((1.13260046146793,1.30781436262561,1.13260046146793))
REPRESENTATION_ITEM('')
);
#217=(
BOUNDED_CURVE()
B_SPLINE_CURVE(2,(#6427,#6428,#6429),.UNSPECIFIED.,.F.,.F.)
B_SPLINE_CURVE_WITH_KNOTS((3,3),(0.137956735689167,0.609258407070138),
 .UNSPECIFIED.)
CURVE()
GEOMETRIC_REPRESENTATION_ITEM()
RATIONAL_B_SPLINE_CURVE((1.13260046146793,1.30781436262561,1.13260046146793))
REPRESENTATION_ITEM('')
);
#218=(
BOUNDED_CURVE()
B_SPLINE_CURVE(2,(#6430,#6431,#6432),.UNSPECIFIED.,.F.,.F.)
B_SPLINE_CURVE_WITH_KNOTS((3,3),(0.137956735689167,0.609258407070138),
 .UNSPECIFIED.)
CURVE()
GEOMETRIC_REPRESENTATION_ITEM()
RATIONAL_B_SPLINE_CURVE((1.13260046146793,1.30781436262561,1.13260046146793))
REPRESENTATION_ITEM('')
);
#219=(
BOUNDED_CURVE()
B_SPLINE_CURVE(2,(#6577,#6578,#6579),.UNSPECIFIED.,.F.,.F.)
B_SPLINE_CURVE_WITH_KNOTS((3,3),(0.140651836354967,0.670383167684795),
 .UNSPECIFIED.)
CURVE()
GEOMETRIC_REPRESENTATION_ITEM()
RATIONAL_B_SPLINE_CURVE((1.11602540378444,1.28867513459481,1.11602540378444))
REPRESENTATION_ITEM('')
);
#220=(
BOUNDED_CURVE()
B_SPLINE_CURVE(2,(#6581,#6582,#6583),.UNSPECIFIED.,.F.,.F.)
B_SPLINE_CURVE_WITH_KNOTS((3,3),(0.140651836354967,0.670383167684795),
 .UNSPECIFIED.)
CURVE()
GEOMETRIC_REPRESENTATION_ITEM()
RATIONAL_B_SPLINE_CURVE((1.11602540378444,1.28867513459481,1.11602540378444))
REPRESENTATION_ITEM('')
);
#221=(
BOUNDED_CURVE()
B_SPLINE_CURVE(2,(#6588,#6589,#6590),.UNSPECIFIED.,.F.,.F.)
B_SPLINE_CURVE_WITH_KNOTS((3,3),(0.140651836354967,0.670383167684795),
 .UNSPECIFIED.)
CURVE()
GEOMETRIC_REPRESENTATION_ITEM()
RATIONAL_B_SPLINE_CURVE((1.11602540378444,1.28867513459481,1.11602540378444))
REPRESENTATION_ITEM('')
);
#222=(
BOUNDED_CURVE()
B_SPLINE_CURVE(2,(#6592,#6593,#6594),.UNSPECIFIED.,.F.,.F.)
B_SPLINE_CURVE_WITH_KNOTS((3,3),(0.140651836354967,0.670383167684795),
 .UNSPECIFIED.)
CURVE()
GEOMETRIC_REPRESENTATION_ITEM()
RATIONAL_B_SPLINE_CURVE((1.11602540378444,1.28867513459481,1.11602540378444))
REPRESENTATION_ITEM('')
);
#223=(
BOUNDED_CURVE()
B_SPLINE_CURVE(2,(#6596,#6597,#6598),.UNSPECIFIED.,.F.,.F.)
B_SPLINE_CURVE_WITH_KNOTS((3,3),(0.140651836354967,0.670383167684795),
 .UNSPECIFIED.)
CURVE()
GEOMETRIC_REPRESENTATION_ITEM()
RATIONAL_B_SPLINE_CURVE((1.11602540378444,1.28867513459481,1.11602540378444))
REPRESENTATION_ITEM('')
);
#224=(
BOUNDED_CURVE()
B_SPLINE_CURVE(2,(#6599,#6600,#6601),.UNSPECIFIED.,.F.,.F.)
B_SPLINE_CURVE_WITH_KNOTS((3,3),(0.140651836354967,0.670383167684795),
 .UNSPECIFIED.)
CURVE()
GEOMETRIC_REPRESENTATION_ITEM()
RATIONAL_B_SPLINE_CURVE((1.11602540378444,1.28867513459481,1.11602540378444))
REPRESENTATION_ITEM('')
);
#225=(
BOUNDED_CURVE()
B_SPLINE_CURVE(2,(#6608,#6609,#6610),.UNSPECIFIED.,.F.,.F.)
B_SPLINE_CURVE_WITH_KNOTS((3,3),(0.140651836354967,0.670383167684795),
 .UNSPECIFIED.)
CURVE()
GEOMETRIC_REPRESENTATION_ITEM()
RATIONAL_B_SPLINE_CURVE((1.11602540378444,1.28867513459481,1.11602540378444))
REPRESENTATION_ITEM('')
);
#226=(
BOUNDED_CURVE()
B_SPLINE_CURVE(2,(#6612,#6613,#6614),.UNSPECIFIED.,.F.,.F.)
B_SPLINE_CURVE_WITH_KNOTS((3,3),(0.140651836354967,0.670383167684796),
 .UNSPECIFIED.)
CURVE()
GEOMETRIC_REPRESENTATION_ITEM()
RATIONAL_B_SPLINE_CURVE((1.11602540378444,1.28867513459481,1.11602540378444))
REPRESENTATION_ITEM('')
);
#227=(
BOUNDED_CURVE()
B_SPLINE_CURVE(2,(#6616,#6617,#6618),.UNSPECIFIED.,.F.,.F.)
B_SPLINE_CURVE_WITH_KNOTS((3,3),(0.140651836354967,0.670383167684795),
 .UNSPECIFIED.)
CURVE()
GEOMETRIC_REPRESENTATION_ITEM()
RATIONAL_B_SPLINE_CURVE((1.11602540378444,1.28867513459481,1.11602540378444))
REPRESENTATION_ITEM('')
);
#228=(
BOUNDED_CURVE()
B_SPLINE_CURVE(2,(#6620,#6621,#6622),.UNSPECIFIED.,.F.,.F.)
B_SPLINE_CURVE_WITH_KNOTS((3,3),(0.140651836354967,0.670383167684795),
 .UNSPECIFIED.)
CURVE()
GEOMETRIC_REPRESENTATION_ITEM()
RATIONAL_B_SPLINE_CURVE((1.11602540378444,1.28867513459482,1.11602540378444))
REPRESENTATION_ITEM('')
);
#229=(
BOUNDED_CURVE()
B_SPLINE_CURVE(2,(#6624,#6625,#6626),.UNSPECIFIED.,.F.,.F.)
B_SPLINE_CURVE_WITH_KNOTS((3,3),(0.140651836354967,0.670383167684795),
 .UNSPECIFIED.)
CURVE()
GEOMETRIC_REPRESENTATION_ITEM()
RATIONAL_B_SPLINE_CURVE((1.11602540378444,1.28867513459481,1.11602540378444))
REPRESENTATION_ITEM('')
);
#230=(
BOUNDED_CURVE()
B_SPLINE_CURVE(2,(#6627,#6628,#6629),.UNSPECIFIED.,.F.,.F.)
B_SPLINE_CURVE_WITH_KNOTS((3,3),(0.140651836354967,0.670383167684795),
 .UNSPECIFIED.)
CURVE()
GEOMETRIC_REPRESENTATION_ITEM()
RATIONAL_B_SPLINE_CURVE((1.11602540378444,1.28867513459481,1.11602540378444))
REPRESENTATION_ITEM('')
);
#231=ORIENTED_CLOSED_SHELL('',*,#3805,.F.);
#232=ORIENTED_CLOSED_SHELL('',*,#3810,.F.);
#233=ORIENTED_CLOSED_SHELL('',*,#3814,.F.);
#234=BREP_WITH_VOIDS('Body1',#3806,(#231));
#235=BREP_WITH_VOIDS('Body1',#3809,(#232));
#236=BREP_WITH_VOIDS('Body1',#3813,(#233));
#237=ELLIPSE('',#4125,0.299389011154384,0.2117);
#238=ELLIPSE('',#4130,0.299389011154384,0.2117);
#239=TOROIDAL_SURFACE('',#4113,0.12,0.08);
#240=CONICAL_SURFACE('',#4092,0.475,0.785398163397448);
#241=CONICAL_SURFACE('',#4100,0.255,0.785398163397449);
#242=CONICAL_SURFACE('',#4153,0.4,0.785398163397448);
#243=CONICAL_SURFACE('',#4157,0.41,0.785398163397448);
#244=CONICAL_SURFACE('',#4161,0.26,0.463647609000806);
#245=CONICAL_SURFACE('',#4212,0.325,0.785398163397448);
#246=CONICAL_SURFACE('',#4216,0.335,0.785398163397448);
#247=CONICAL_SURFACE('',#4220,0.21,0.463647609000806);
#248=CONICAL_SURFACE('',#4224,0.18,0.785398163397448);
#249=CONICAL_SURFACE('',#4236,0.418322594216369,1.0471975511966);
#250=CONICAL_SURFACE('',#4238,0.418322594216369,1.0471975511966);
#251=CONICAL_SURFACE('',#4252,0.275,0.785398163397449);
#252=CONICAL_SURFACE('',#4296,0.4,0.785398163397448);
#253=CONICAL_SURFACE('',#4300,0.41,0.785398163397448);
#254=CONICAL_SURFACE('',#4304,0.26,0.463647609000806);
#255=CONICAL_SURFACE('',#4308,0.225,0.785398163397448);
#256=CONICAL_SURFACE('',#4320,0.47094010767585,1.0471975511966);
#257=CONICAL_SURFACE('',#4322,0.47094010767585,1.0471975511966);
#258=B_SPLINE_CURVE_WITH_KNOTS('',3,(#5867,#5868,#5869,#5870,#5871,#5872,
#5873,#5874,#5875,#5876),.UNSPECIFIED.,.F.,.F.,(4,2,2,2,4),(0.,0.0302963256060356,
0.0605926512120712,0.090883446720838,0.121174242229605),.UNSPECIFIED.);
#259=B_SPLINE_CURVE_WITH_KNOTS('',3,(#5879,#5880,#5881,#5882,#5883,#5884,
#5885,#5886,#5887,#5888,#5889,#5890,#5891,#5892,#5893,#5894,#5895,#5896,
#5897,#5898,#5899,#5900,#5901,#5902,#5903,#5904,#5905,#5906,#5907,#5908,
#5909,#5910,#5911,#5912),.UNSPECIFIED.,.T.,.F.,(4,2,2,2,2,2,2,2,2,2,2,2,
2,2,2,2,4),(0.,0.0302963256060358,0.0605926512120716,0.0908834467208383,
0.121174242229605,0.151465037738372,0.181755833247138,0.212052158853174,
0.24234848445921,0.272644810065246,0.302941135671282,0.333231931180048,
0.363522726688815,0.393813522197582,0.424104317706349,0.454400643312384,
0.48469696891842),.UNSPECIFIED.);
#260=B_SPLINE_CURVE_WITH_KNOTS('',3,(#5914,#5915,#5916,#5917,#5918,#5919,
#5920,#5921,#5922,#5923),.UNSPECIFIED.,.F.,.F.,(4,2,2,2,4),(0.363522726688815,
0.393813522197581,0.424104317706348,0.454400643312384,0.48469696891842),
 .UNSPECIFIED.);
#261=B_SPLINE_CURVE_WITH_KNOTS('',3,(#5924,#5925,#5926,#5927,#5928,#5929,
#5930,#5931,#5932,#5933,#5934,#5935,#5936,#5937,#5938,#5939,#5940,#5941),
 .UNSPECIFIED.,.F.,.F.,(4,2,2,2,2,2,2,2,4),(0.121174242229605,0.151465037738371,
0.181755833247138,0.212052158853174,0.24234848445921,0.272644810065246,
0.302941135671281,0.333231931180048,0.363522726688815),.UNSPECIFIED.);
#262=B_SPLINE_CURVE_WITH_KNOTS('',3,(#5988,#5989,#5990,#5991,#5992,#5993,
#5994,#5995,#5996,#5997,#5998,#5999,#6000,#6001,#6002,#6003,#6004,#6005,
#6006,#6007,#6008,#6009,#6010,#6011,#6012,#6013),.UNSPECIFIED.,.F.,.F.,
(4,2,2,2,2,2,2,2,2,2,2,2,4),(-0.00054581412719389,0.,0.0281583564005144,
0.0618496465371181,0.0905865724114538,0.120694112793616,0.144966158459363,
0.16923820412511,0.199345744507272,0.228082670381608,0.261773960518212,
0.289932316918681,0.290478131045882),.UNSPECIFIED.);
#263=B_SPLINE_CURVE_WITH_KNOTS('',3,(#6014,#6015,#6016,#6017,#6018,#6019,
#6020,#6021,#6022,#6023,#6024,#6025,#6026,#6027,#6028,#6029,#6030,#6031,
#6032,#6033,#6034,#6035,#6036,#6037,#6038,#6039),.UNSPECIFIED.,.F.,.F.,
(4,2,2,2,2,2,2,2,2,2,2,2,4),(-0.000545814127196571,0.,0.0281583564006391,
0.0618496465374156,0.0905865724118984,0.120694112794215,0.144966158460086,
0.169238204125958,0.199345744508275,0.228082670382758,0.261773960519534,
0.289932316920171,0.29047813104737),.UNSPECIFIED.);
#264=SHAPE_REPRESENTATION_RELATIONSHIP('SRR','None',#6839,#280);
#265=SHAPE_REPRESENTATION_RELATIONSHIP('SRR','None',#6840,#281);
#266=SHAPE_REPRESENTATION_RELATIONSHIP('SRR','None',#6841,#282);
#267=SHAPE_REPRESENTATION_RELATIONSHIP('SRR','None',#6842,#283);
#268=SHAPE_REPRESENTATION_RELATIONSHIP('SRR','None',#6843,#284);
#269=SHAPE_REPRESENTATION_RELATIONSHIP('SRR','None',#6844,#285);
#270=SHAPE_REPRESENTATION_RELATIONSHIP('SRR','None',#6845,#286);
#271=SHAPE_REPRESENTATION_RELATIONSHIP('SRR','None',#6846,#287);
#272=SHAPE_REPRESENTATION_RELATIONSHIP('SRR','None',#6848,#288);
#273=SHAPE_REPRESENTATION_RELATIONSHIP('SRR','None',#6849,#289);
#274=SHAPE_REPRESENTATION_RELATIONSHIP('SRR','None',#6850,#290);
#275=SHAPE_REPRESENTATION_RELATIONSHIP('SRR','None',#6851,#291);
#276=SHAPE_REPRESENTATION_RELATIONSHIP('SRR','None',#6852,#292);
#277=SHAPE_REPRESENTATION_RELATIONSHIP('SRR','None',#6853,#293);
#278=SHAPE_REPRESENTATION_RELATIONSHIP('SRR','None',#6854,#294);
#279=SHAPE_REPRESENTATION_RELATIONSHIP('SRR','None',#6856,#295);
#280=ADVANCED_BREP_SHAPE_REPRESENTATION('',(#312),#6725);
#281=ADVANCED_BREP_SHAPE_REPRESENTATION('',(#313),#6726);
#282=ADVANCED_BREP_SHAPE_REPRESENTATION('',(#314),#6727);
#283=ADVANCED_BREP_SHAPE_REPRESENTATION('',(#315),#6728);
#284=ADVANCED_BREP_SHAPE_REPRESENTATION('',(#316),#6729);
#285=ADVANCED_BREP_SHAPE_REPRESENTATION('',(#317),#6730);
#286=ADVANCED_BREP_SHAPE_REPRESENTATION('',(#318),#6731);
#287=ADVANCED_BREP_SHAPE_REPRESENTATION('',(#234),#6732);
#288=ADVANCED_BREP_SHAPE_REPRESENTATION('',(#319),#6734);
#289=ADVANCED_BREP_SHAPE_REPRESENTATION('',(#320),#6735);
#290=ADVANCED_BREP_SHAPE_REPRESENTATION('',(#235),#6736);
#291=ADVANCED_BREP_SHAPE_REPRESENTATION('',(#321),#6737);
#292=ADVANCED_BREP_SHAPE_REPRESENTATION('',(#322),#6738);
#293=ADVANCED_BREP_SHAPE_REPRESENTATION('',(#236),#6739);
#294=ADVANCED_BREP_SHAPE_REPRESENTATION('',(#323),#6740);
#295=ADVANCED_BREP_SHAPE_REPRESENTATION('',(#324),#6742);
#296=STYLED_ITEM('',(#6989),#312);
#297=STYLED_ITEM('',(#7017),#313);
#298=STYLED_ITEM('',(#6989),#314);
#299=STYLED_ITEM('',(#7003),#315);
#300=STYLED_ITEM('',(#7010),#316);
#301=STYLED_ITEM('',(#7003),#317);
#302=STYLED_ITEM('',(#7010),#318);
#303=STYLED_ITEM('',(#7010),#234);
#304=STYLED_ITEM('',(#6989),#319);
#305=STYLED_ITEM('',(#6989),#320);
#306=STYLED_ITEM('',(#7010),#235);
#307=STYLED_ITEM('',(#7010),#321);
#308=STYLED_ITEM('',(#7010),#322);
#309=STYLED_ITEM('',(#7010),#236);
#310=STYLED_ITEM('',(#7010),#323);
#311=STYLED_ITEM('',(#6989),#324);
#312=MANIFOLD_SOLID_BREP('Body1',#3798);
#313=MANIFOLD_SOLID_BREP('Body1',#3799);
#314=MANIFOLD_SOLID_BREP('Body1',#3800);
#315=MANIFOLD_SOLID_BREP('Body1',#3801);
#316=MANIFOLD_SOLID_BREP('Body1',#3802);
#317=MANIFOLD_SOLID_BREP('Body1',#3803);
#318=MANIFOLD_SOLID_BREP('Body1',#3804);
#319=MANIFOLD_SOLID_BREP('Body1',#3807);
#320=MANIFOLD_SOLID_BREP('Body1',#3808);
#321=MANIFOLD_SOLID_BREP('Body1',#3811);
#322=MANIFOLD_SOLID_BREP('Body1',#3812);
#323=MANIFOLD_SOLID_BREP('Body1',#3815);
#324=MANIFOLD_SOLID_BREP('Body1',#3816);
#325=FACE_BOUND('',#732,.T.);
#326=FACE_BOUND('',#733,.T.);
#327=FACE_BOUND('',#736,.T.);
#328=FACE_BOUND('',#737,.T.);
#329=FACE_BOUND('',#787,.T.);
#330=FACE_BOUND('',#789,.T.);
#331=FACE_BOUND('',#797,.T.);
#332=FACE_BOUND('',#798,.T.);
#333=FACE_BOUND('',#801,.T.);
#334=FACE_BOUND('',#804,.T.);
#335=FACE_BOUND('',#807,.T.);
#336=FACE_BOUND('',#809,.T.);
#337=FACE_BOUND('',#810,.T.);
#338=FACE_BOUND('',#813,.T.);
#339=FACE_BOUND('',#819,.T.);
#340=FACE_BOUND('',#821,.T.);
#341=FACE_BOUND('',#827,.T.);
#342=FACE_BOUND('',#829,.T.);
#343=FACE_BOUND('',#831,.T.);
#344=FACE_BOUND('',#846,.T.);
#345=FACE_BOUND('',#861,.T.);
#346=FACE_BOUND('',#870,.T.);
#347=FACE_BOUND('',#871,.T.);
#348=FACE_BOUND('',#872,.T.);
#349=FACE_BOUND('',#873,.T.);
#350=FACE_BOUND('',#874,.T.);
#351=FACE_BOUND('',#877,.T.);
#352=FACE_BOUND('',#878,.T.);
#353=FACE_BOUND('',#879,.T.);
#354=FACE_BOUND('',#880,.T.);
#355=FACE_BOUND('',#881,.T.);
#356=FACE_BOUND('',#894,.T.);
#357=FACE_BOUND('',#896,.T.);
#358=FACE_BOUND('',#897,.T.);
#359=FACE_BOUND('',#899,.T.);
#360=FACE_BOUND('',#900,.T.);
#361=FACE_BOUND('',#903,.T.);
#362=FACE_BOUND('',#909,.T.);
#363=FACE_BOUND('',#932,.T.);
#364=FACE_BOUND('',#934,.T.);
#365=FACE_BOUND('',#938,.T.);
#366=FACE_BOUND('',#941,.T.);
#367=FACE_BOUND('',#947,.T.);
#368=FACE_BOUND('',#970,.T.);
#369=FACE_BOUND('',#972,.T.);
#370=FACE_BOUND('',#975,.T.);
#371=FACE_BOUND('',#978,.T.);
#372=PLANE('',#4003);
#373=PLANE('',#4004);
#374=PLANE('',#4005);
#375=PLANE('',#4006);
#376=PLANE('',#4007);
#377=PLANE('',#4008);
#378=PLANE('',#4010);
#379=PLANE('',#4011);
#380=PLANE('',#4012);
#381=PLANE('',#4013);
#382=PLANE('',#4014);
#383=PLANE('',#4015);
#384=PLANE('',#4016);
#385=PLANE('',#4017);
#386=PLANE('',#4018);
#387=PLANE('',#4019);
#388=PLANE('',#4020);
#389=PLANE('',#4021);
#390=PLANE('',#4022);
#391=PLANE('',#4023);
#392=PLANE('',#4024);
#393=PLANE('',#4025);
#394=PLANE('',#4026);
#395=PLANE('',#4027);
#396=PLANE('',#4028);
#397=PLANE('',#4029);
#398=PLANE('',#4030);
#399=PLANE('',#4031);
#400=PLANE('',#4032);
#401=PLANE('',#4033);
#402=PLANE('',#4034);
#403=PLANE('',#4035);
#404=PLANE('',#4036);
#405=PLANE('',#4037);
#406=PLANE('',#4038);
#407=PLANE('',#4039);
#408=PLANE('',#4040);
#409=PLANE('',#4041);
#410=PLANE('',#4042);
#411=PLANE('',#4043);
#412=PLANE('',#4044);
#413=PLANE('',#4045);
#414=PLANE('',#4049);
#415=PLANE('',#4050);
#416=PLANE('',#4051);
#417=PLANE('',#4052);
#418=PLANE('',#4053);
#419=PLANE('',#4054);
#420=PLANE('',#4055);
#421=PLANE('',#4056);
#422=PLANE('',#4057);
#423=PLANE('',#4058);
#424=PLANE('',#4072);
#425=PLANE('',#4073);
#426=PLANE('',#4074);
#427=PLANE('',#4078);
#428=PLANE('',#4079);
#429=PLANE('',#4080);
#430=PLANE('',#4084);
#431=PLANE('',#4085);
#432=PLANE('',#4086);
#433=PLANE('',#4087);
#434=PLANE('',#4090);
#435=PLANE('',#4096);
#436=PLANE('',#4102);
#437=PLANE('',#4110);
#438=PLANE('',#4111);
#439=PLANE('',#4116);
#440=PLANE('',#4118);
#441=PLANE('',#4122);
#442=PLANE('',#4124);
#443=PLANE('',#4132);
#444=PLANE('',#4133);
#445=PLANE('',#4134);
#446=PLANE('',#4135);
#447=PLANE('',#4136);
#448=PLANE('',#4137);
#449=PLANE('',#4138);
#450=PLANE('',#4139);
#451=PLANE('',#4141);
#452=PLANE('',#4142);
#453=PLANE('',#4143);
#454=PLANE('',#4144);
#455=PLANE('',#4145);
#456=PLANE('',#4146);
#457=PLANE('',#4147);
#458=PLANE('',#4148);
#459=PLANE('',#4149);
#460=PLANE('',#4151);
#461=PLANE('',#4159);
#462=PLANE('',#4181);
#463=PLANE('',#4182);
#464=PLANE('',#4183);
#465=PLANE('',#4184);
#466=PLANE('',#4185);
#467=PLANE('',#4186);
#468=PLANE('',#4197);
#469=PLANE('',#4198);
#470=PLANE('',#4199);
#471=PLANE('',#4200);
#472=PLANE('',#4201);
#473=PLANE('',#4202);
#474=PLANE('',#4204);
#475=PLANE('',#4205);
#476=PLANE('',#4208);
#477=PLANE('',#4210);
#478=PLANE('',#4218);
#479=PLANE('',#4226);
#480=PLANE('',#4227);
#481=PLANE('',#4228);
#482=PLANE('',#4229);
#483=PLANE('',#4230);
#484=PLANE('',#4231);
#485=PLANE('',#4232);
#486=PLANE('',#4233);
#487=PLANE('',#4234);
#488=PLANE('',#4240);
#489=PLANE('',#4241);
#490=PLANE('',#4242);
#491=PLANE('',#4246);
#492=PLANE('',#4247);
#493=PLANE('',#4248);
#494=PLANE('',#4249);
#495=PLANE('',#4250);
#496=PLANE('',#4257);
#497=PLANE('',#4261);
#498=PLANE('',#4294);
#499=PLANE('',#4302);
#500=PLANE('',#4310);
#501=PLANE('',#4311);
#502=PLANE('',#4312);
#503=PLANE('',#4313);
#504=PLANE('',#4314);
#505=PLANE('',#4315);
#506=PLANE('',#4316);
#507=PLANE('',#4317);
#508=PLANE('',#4318);
#509=PLANE('',#4324);
#510=PLANE('',#4325);
#511=PLANE('',#4326);
#512=PLANE('',#4330);
#513=PLANE('',#4331);
#514=PLANE('',#4332);
#515=PLANE('',#4333);
#516=PLANE('',#4334);
#517=PLANE('',#4354);
#518=PLANE('',#4355);
#519=PLANE('',#4356);
#520=PLANE('',#4357);
#521=PLANE('',#4358);
#522=PLANE('',#4359);
#523=FACE_OUTER_BOUND('',#729,.T.);
#524=FACE_OUTER_BOUND('',#730,.T.);
#525=FACE_OUTER_BOUND('',#731,.T.);
#526=FACE_OUTER_BOUND('',#734,.T.);
#527=FACE_OUTER_BOUND('',#735,.T.);
#528=FACE_OUTER_BOUND('',#738,.T.);
#529=FACE_OUTER_BOUND('',#739,.T.);
#530=FACE_OUTER_BOUND('',#740,.T.);
#531=FACE_OUTER_BOUND('',#741,.T.);
#532=FACE_OUTER_BOUND('',#742,.T.);
#533=FACE_OUTER_BOUND('',#743,.T.);
#534=FACE_OUTER_BOUND('',#744,.T.);
#535=FACE_OUTER_BOUND('',#745,.T.);
#536=FACE_OUTER_BOUND('',#746,.T.);
#537=FACE_OUTER_BOUND('',#747,.T.);
#538=FACE_OUTER_BOUND('',#748,.T.);
#539=FACE_OUTER_BOUND('',#749,.T.);
#540=FACE_OUTER_BOUND('',#750,.T.);
#541=FACE_OUTER_BOUND('',#751,.T.);
#542=FACE_OUTER_BOUND('',#752,.T.);
#543=FACE_OUTER_BOUND('',#753,.T.);
#544=FACE_OUTER_BOUND('',#754,.T.);
#545=FACE_OUTER_BOUND('',#755,.T.);
#546=FACE_OUTER_BOUND('',#756,.T.);
#547=FACE_OUTER_BOUND('',#757,.T.);
#548=FACE_OUTER_BOUND('',#758,.T.);
#549=FACE_OUTER_BOUND('',#759,.T.);
#550=FACE_OUTER_BOUND('',#760,.T.);
#551=FACE_OUTER_BOUND('',#761,.T.);
#552=FACE_OUTER_BOUND('',#762,.T.);
#553=FACE_OUTER_BOUND('',#763,.T.);
#554=FACE_OUTER_BOUND('',#764,.T.);
#555=FACE_OUTER_BOUND('',#765,.T.);
#556=FACE_OUTER_BOUND('',#766,.T.);
#557=FACE_OUTER_BOUND('',#767,.T.);
#558=FACE_OUTER_BOUND('',#768,.T.);
#559=FACE_OUTER_BOUND('',#769,.T.);
#560=FACE_OUTER_BOUND('',#770,.T.);
#561=FACE_OUTER_BOUND('',#771,.T.);
#562=FACE_OUTER_BOUND('',#772,.T.);
#563=FACE_OUTER_BOUND('',#773,.T.);
#564=FACE_OUTER_BOUND('',#774,.T.);
#565=FACE_OUTER_BOUND('',#775,.T.);
#566=FACE_OUTER_BOUND('',#776,.T.);
#567=FACE_OUTER_BOUND('',#777,.T.);
#568=FACE_OUTER_BOUND('',#778,.T.);
#569=FACE_OUTER_BOUND('',#779,.T.);
#570=FACE_OUTER_BOUND('',#780,.T.);
#571=FACE_OUTER_BOUND('',#781,.T.);
#572=FACE_OUTER_BOUND('',#782,.T.);
#573=FACE_OUTER_BOUND('',#783,.T.);
#574=FACE_OUTER_BOUND('',#784,.T.);
#575=FACE_OUTER_BOUND('',#785,.T.);
#576=FACE_OUTER_BOUND('',#786,.T.);
#577=FACE_OUTER_BOUND('',#788,.T.);
#578=FACE_OUTER_BOUND('',#790,.T.);
#579=FACE_OUTER_BOUND('',#791,.T.);
#580=FACE_OUTER_BOUND('',#792,.T.);
#581=FACE_OUTER_BOUND('',#793,.T.);
#582=FACE_OUTER_BOUND('',#794,.T.);
#583=FACE_OUTER_BOUND('',#795,.T.);
#584=FACE_OUTER_BOUND('',#796,.T.);
#585=FACE_OUTER_BOUND('',#799,.T.);
#586=FACE_OUTER_BOUND('',#800,.T.);
#587=FACE_OUTER_BOUND('',#802,.T.);
#588=FACE_OUTER_BOUND('',#803,.T.);
#589=FACE_OUTER_BOUND('',#805,.T.);
#590=FACE_OUTER_BOUND('',#806,.T.);
#591=FACE_OUTER_BOUND('',#808,.T.);
#592=FACE_OUTER_BOUND('',#811,.T.);
#593=FACE_OUTER_BOUND('',#812,.T.);
#594=FACE_OUTER_BOUND('',#814,.T.);
#595=FACE_OUTER_BOUND('',#815,.T.);
#596=FACE_OUTER_BOUND('',#816,.T.);
#597=FACE_OUTER_BOUND('',#817,.T.);
#598=FACE_OUTER_BOUND('',#818,.T.);
#599=FACE_OUTER_BOUND('',#820,.T.);
#600=FACE_OUTER_BOUND('',#822,.T.);
#601=FACE_OUTER_BOUND('',#823,.T.);
#602=FACE_OUTER_BOUND('',#824,.T.);
#603=FACE_OUTER_BOUND('',#825,.T.);
#604=FACE_OUTER_BOUND('',#826,.T.);
#605=FACE_OUTER_BOUND('',#828,.T.);
#606=FACE_OUTER_BOUND('',#830,.T.);
#607=FACE_OUTER_BOUND('',#832,.T.);
#608=FACE_OUTER_BOUND('',#833,.T.);
#609=FACE_OUTER_BOUND('',#834,.T.);
#610=FACE_OUTER_BOUND('',#835,.T.);
#611=FACE_OUTER_BOUND('',#836,.T.);
#612=FACE_OUTER_BOUND('',#837,.T.);
#613=FACE_OUTER_BOUND('',#838,.T.);
#614=FACE_OUTER_BOUND('',#839,.T.);
#615=FACE_OUTER_BOUND('',#840,.T.);
#616=FACE_OUTER_BOUND('',#841,.T.);
#617=FACE_OUTER_BOUND('',#842,.T.);
#618=FACE_OUTER_BOUND('',#843,.T.);
#619=FACE_OUTER_BOUND('',#844,.T.);
#620=FACE_OUTER_BOUND('',#845,.T.);
#621=FACE_OUTER_BOUND('',#847,.T.);
#622=FACE_OUTER_BOUND('',#848,.T.);
#623=FACE_OUTER_BOUND('',#849,.T.);
#624=FACE_OUTER_BOUND('',#850,.T.);
#625=FACE_OUTER_BOUND('',#851,.T.);
#626=FACE_OUTER_BOUND('',#852,.T.);
#627=FACE_OUTER_BOUND('',#853,.T.);
#628=FACE_OUTER_BOUND('',#854,.T.);
#629=FACE_OUTER_BOUND('',#855,.T.);
#630=FACE_OUTER_BOUND('',#856,.T.);
#631=FACE_OUTER_BOUND('',#857,.T.);
#632=FACE_OUTER_BOUND('',#858,.T.);
#633=FACE_OUTER_BOUND('',#859,.T.);
#634=FACE_OUTER_BOUND('',#860,.T.);
#635=FACE_OUTER_BOUND('',#862,.T.);
#636=FACE_OUTER_BOUND('',#863,.T.);
#637=FACE_OUTER_BOUND('',#864,.T.);
#638=FACE_OUTER_BOUND('',#865,.T.);
#639=FACE_OUTER_BOUND('',#866,.T.);
#640=FACE_OUTER_BOUND('',#867,.T.);
#641=FACE_OUTER_BOUND('',#868,.T.);
#642=FACE_OUTER_BOUND('',#869,.T.);
#643=FACE_OUTER_BOUND('',#875,.T.);
#644=FACE_OUTER_BOUND('',#876,.T.);
#645=FACE_OUTER_BOUND('',#882,.T.);
#646=FACE_OUTER_BOUND('',#883,.T.);
#647=FACE_OUTER_BOUND('',#884,.T.);
#648=FACE_OUTER_BOUND('',#885,.T.);
#649=FACE_OUTER_BOUND('',#886,.T.);
#650=FACE_OUTER_BOUND('',#887,.T.);
#651=FACE_OUTER_BOUND('',#888,.T.);
#652=FACE_OUTER_BOUND('',#889,.T.);
#653=FACE_OUTER_BOUND('',#890,.T.);
#654=FACE_OUTER_BOUND('',#891,.T.);
#655=FACE_OUTER_BOUND('',#892,.T.);
#656=FACE_OUTER_BOUND('',#893,.T.);
#657=FACE_OUTER_BOUND('',#895,.T.);
#658=FACE_OUTER_BOUND('',#898,.T.);
#659=FACE_OUTER_BOUND('',#901,.T.);
#660=FACE_OUTER_BOUND('',#902,.T.);
#661=FACE_OUTER_BOUND('',#904,.T.);
#662=FACE_OUTER_BOUND('',#905,.T.);
#663=FACE_OUTER_BOUND('',#906,.T.);
#664=FACE_OUTER_BOUND('',#907,.T.);
#665=FACE_OUTER_BOUND('',#908,.T.);
#666=FACE_OUTER_BOUND('',#910,.T.);
#667=FACE_OUTER_BOUND('',#911,.T.);
#668=FACE_OUTER_BOUND('',#912,.T.);
#669=FACE_OUTER_BOUND('',#913,.T.);
#670=FACE_OUTER_BOUND('',#914,.T.);
#671=FACE_OUTER_BOUND('',#915,.T.);
#672=FACE_OUTER_BOUND('',#916,.T.);
#673=FACE_OUTER_BOUND('',#917,.T.);
#674=FACE_OUTER_BOUND('',#918,.T.);
#675=FACE_OUTER_BOUND('',#919,.T.);
#676=FACE_OUTER_BOUND('',#920,.T.);
#677=FACE_OUTER_BOUND('',#921,.T.);
#678=FACE_OUTER_BOUND('',#922,.T.);
#679=FACE_OUTER_BOUND('',#923,.T.);
#680=FACE_OUTER_BOUND('',#924,.T.);
#681=FACE_OUTER_BOUND('',#925,.T.);
#682=FACE_OUTER_BOUND('',#926,.T.);
#683=FACE_OUTER_BOUND('',#927,.T.);
#684=FACE_OUTER_BOUND('',#928,.T.);
#685=FACE_OUTER_BOUND('',#929,.T.);
#686=FACE_OUTER_BOUND('',#930,.T.);
#687=FACE_OUTER_BOUND('',#931,.T.);
#688=FACE_OUTER_BOUND('',#933,.T.);
#689=FACE_OUTER_BOUND('',#935,.T.);
#690=FACE_OUTER_BOUND('',#936,.T.);
#691=FACE_OUTER_BOUND('',#937,.T.);
#692=FACE_OUTER_BOUND('',#939,.T.);
#693=FACE_OUTER_BOUND('',#940,.T.);
#694=FACE_OUTER_BOUND('',#942,.T.);
#695=FACE_OUTER_BOUND('',#943,.T.);
#696=FACE_OUTER_BOUND('',#944,.T.);
#697=FACE_OUTER_BOUND('',#945,.T.);
#698=FACE_OUTER_BOUND('',#946,.T.);
#699=FACE_OUTER_BOUND('',#948,.T.);
#700=FACE_OUTER_BOUND('',#949,.T.);
#701=FACE_OUTER_BOUND('',#950,.T.);
#702=FACE_OUTER_BOUND('',#951,.T.);
#703=FACE_OUTER_BOUND('',#952,.T.);
#704=FACE_OUTER_BOUND('',#953,.T.);
#705=FACE_OUTER_BOUND('',#954,.T.);
#706=FACE_OUTER_BOUND('',#955,.T.);
#707=FACE_OUTER_BOUND('',#956,.T.);
#708=FACE_OUTER_BOUND('',#957,.T.);
#709=FACE_OUTER_BOUND('',#958,.T.);
#710=FACE_OUTER_BOUND('',#959,.T.);
#711=FACE_OUTER_BOUND('',#960,.T.);
#712=FACE_OUTER_BOUND('',#961,.T.);
#713=FACE_OUTER_BOUND('',#962,.T.);
#714=FACE_OUTER_BOUND('',#963,.T.);
#715=FACE_OUTER_BOUND('',#964,.T.);
#716=FACE_OUTER_BOUND('',#965,.T.);
#717=FACE_OUTER_BOUND('',#966,.T.);
#718=FACE_OUTER_BOUND('',#967,.T.);
#719=FACE_OUTER_BOUND('',#968,.T.);
#720=FACE_OUTER_BOUND('',#969,.T.);
#721=FACE_OUTER_BOUND('',#971,.T.);
#722=FACE_OUTER_BOUND('',#973,.T.);
#723=FACE_OUTER_BOUND('',#974,.T.);
#724=FACE_OUTER_BOUND('',#976,.T.);
#725=FACE_OUTER_BOUND('',#977,.T.);
#726=FACE_OUTER_BOUND('',#979,.T.);
#727=FACE_OUTER_BOUND('',#980,.T.);
#728=FACE_OUTER_BOUND('',#981,.T.);
#729=EDGE_LOOP('',(#2590,#2591,#2592,#2593));
#730=EDGE_LOOP('',(#2594,#2595,#2596,#2597));
#731=EDGE_LOOP('',(#2598,#2599,#2600,#2601));
#732=EDGE_LOOP('',(#2602));
#733=EDGE_LOOP('',(#2603));
#734=EDGE_LOOP('',(#2604,#2605,#2606,#2607));
#735=EDGE_LOOP('',(#2608,#2609,#2610,#2611));
#736=EDGE_LOOP('',(#2612));
#737=EDGE_LOOP('',(#2613));
#738=EDGE_LOOP('',(#2614,#2615,#2616,#2617));
#739=EDGE_LOOP('',(#2618,#2619,#2620,#2621));
#740=EDGE_LOOP('',(#2622,#2623,#2624,#2625));
#741=EDGE_LOOP('',(#2626,#2627,#2628,#2629));
#742=EDGE_LOOP('',(#2630,#2631,#2632,#2633));
#743=EDGE_LOOP('',(#2634,#2635,#2636,#2637));
#744=EDGE_LOOP('',(#2638,#2639,#2640,#2641));
#745=EDGE_LOOP('',(#2642,#2643,#2644,#2645));
#746=EDGE_LOOP('',(#2646,#2647,#2648,#2649));
#747=EDGE_LOOP('',(#2650,#2651,#2652,#2653));
#748=EDGE_LOOP('',(#2654,#2655,#2656,#2657));
#749=EDGE_LOOP('',(#2658,#2659,#2660,#2661));
#750=EDGE_LOOP('',(#2662,#2663,#2664,#2665));
#751=EDGE_LOOP('',(#2666,#2667,#2668,#2669));
#752=EDGE_LOOP('',(#2670,#2671,#2672,#2673));
#753=EDGE_LOOP('',(#2674,#2675,#2676,#2677));
#754=EDGE_LOOP('',(#2678,#2679,#2680,#2681));
#755=EDGE_LOOP('',(#2682,#2683,#2684,#2685));
#756=EDGE_LOOP('',(#2686,#2687,#2688,#2689));
#757=EDGE_LOOP('',(#2690,#2691,#2692,#2693));
#758=EDGE_LOOP('',(#2694,#2695,#2696,#2697));
#759=EDGE_LOOP('',(#2698,#2699,#2700,#2701));
#760=EDGE_LOOP('',(#2702,#2703,#2704,#2705));
#761=EDGE_LOOP('',(#2706,#2707,#2708,#2709));
#762=EDGE_LOOP('',(#2710,#2711,#2712,#2713));
#763=EDGE_LOOP('',(#2714,#2715,#2716,#2717));
#764=EDGE_LOOP('',(#2718,#2719,#2720,#2721));
#765=EDGE_LOOP('',(#2722,#2723,#2724,#2725));
#766=EDGE_LOOP('',(#2726,#2727,#2728,#2729));
#767=EDGE_LOOP('',(#2730,#2731,#2732,#2733));
#768=EDGE_LOOP('',(#2734,#2735,#2736,#2737));
#769=EDGE_LOOP('',(#2738,#2739,#2740,#2741));
#770=EDGE_LOOP('',(#2742,#2743,#2744,#2745));
#771=EDGE_LOOP('',(#2746,#2747,#2748,#2749));
#772=EDGE_LOOP('',(#2750,#2751,#2752,#2753));
#773=EDGE_LOOP('',(#2754,#2755,#2756,#2757));
#774=EDGE_LOOP('',(#2758,#2759,#2760,#2761));
#775=EDGE_LOOP('',(#2762,#2763,#2764,#2765));
#776=EDGE_LOOP('',(#2766,#2767,#2768,#2769));
#777=EDGE_LOOP('',(#2770,#2771,#2772,#2773));
#778=EDGE_LOOP('',(#2774,#2775,#2776,#2777));
#779=EDGE_LOOP('',(#2778,#2779,#2780,#2781));
#780=EDGE_LOOP('',(#2782,#2783,#2784,#2785));
#781=EDGE_LOOP('',(#2786,#2787,#2788,#2789));
#782=EDGE_LOOP('',(#2790,#2791,#2792,#2793));
#783=EDGE_LOOP('',(#2794,#2795,#2796,#2797));
#784=EDGE_LOOP('',(#2798,#2799,#2800,#2801));
#785=EDGE_LOOP('',(#2802,#2803,#2804,#2805));
#786=EDGE_LOOP('',(#2806,#2807,#2808,#2809,#2810,#2811,#2812,#2813,#2814,
#2815,#2816,#2817,#2818,#2819,#2820,#2821,#2822,#2823,#2824,#2825,#2826,
#2827,#2828,#2829,#2830,#2831,#2832,#2833,#2834,#2835,#2836,#2837,#2838,
#2839,#2840,#2841,#2842,#2843,#2844,#2845,#2846,#2847,#2848,#2849));
#787=EDGE_LOOP('',(#2850));
#788=EDGE_LOOP('',(#2851,#2852,#2853,#2854,#2855,#2856,#2857,#2858,#2859,
#2860,#2861,#2862,#2863,#2864,#2865,#2866,#2867,#2868,#2869,#2870,#2871,
#2872,#2873,#2874,#2875,#2876,#2877,#2878,#2879,#2880,#2881,#2882,#2883,
#2884,#2885,#2886,#2887,#2888,#2889,#2890,#2891,#2892,#2893,#2894));
#789=EDGE_LOOP('',(#2895));
#790=EDGE_LOOP('',(#2896,#2897,#2898,#2899));
#791=EDGE_LOOP('',(#2900,#2901,#2902,#2903));
#792=EDGE_LOOP('',(#2904,#2905,#2906,#2907));
#793=EDGE_LOOP('',(#2908,#2909,#2910,#2911));
#794=EDGE_LOOP('',(#2912,#2913,#2914,#2915));
#795=EDGE_LOOP('',(#2916,#2917,#2918,#2919));
#796=EDGE_LOOP('',(#2920,#2921,#2922,#2923,#2924,#2925,#2926,#2927));
#797=EDGE_LOOP('',(#2928));
#798=EDGE_LOOP('',(#2929));
#799=EDGE_LOOP('',(#2930,#2931,#2932,#2933));
#800=EDGE_LOOP('',(#2934,#2935,#2936,#2937,#2938));
#801=EDGE_LOOP('',(#2939));
#802=EDGE_LOOP('',(#2940,#2941,#2942,#2943,#2944,#2945,#2946,#2947));
#803=EDGE_LOOP('',(#2948,#2949,#2950,#2951,#2952));
#804=EDGE_LOOP('',(#2953));
#805=EDGE_LOOP('',(#2954,#2955,#2956,#2957));
#806=EDGE_LOOP('',(#2958,#2959,#2960,#2961,#2962));
#807=EDGE_LOOP('',(#2963));
#808=EDGE_LOOP('',(#2964,#2965,#2966,#2967));
#809=EDGE_LOOP('',(#2968));
#810=EDGE_LOOP('',(#2969));
#811=EDGE_LOOP('',(#2970,#2971,#2972,#2973));
#812=EDGE_LOOP('',(#2974,#2975,#2976,#2977,#2978));
#813=EDGE_LOOP('',(#2979));
#814=EDGE_LOOP('',(#2980,#2981,#2982,#2983,#2984,#2985));
#815=EDGE_LOOP('',(#2986));
#816=EDGE_LOOP('',(#2987,#2988,#2989,#2990));
#817=EDGE_LOOP('',(#2991,#2992,#2993,#2994));
#818=EDGE_LOOP('',(#2995));
#819=EDGE_LOOP('',(#2996));
#820=EDGE_LOOP('',(#2997,#2998,#2999,#3000,#3001,#3002,#3003,#3004,#3005));
#821=EDGE_LOOP('',(#3006));
#822=EDGE_LOOP('',(#3007,#3008,#3009,#3010));
#823=EDGE_LOOP('',(#3011));
#824=EDGE_LOOP('',(#3012,#3013,#3014,#3015));
#825=EDGE_LOOP('',(#3016,#3017,#3018,#3019));
#826=EDGE_LOOP('',(#3020));
#827=EDGE_LOOP('',(#3021));
#828=EDGE_LOOP('',(#3022));
#829=EDGE_LOOP('',(#3023));
#830=EDGE_LOOP('',(#3024,#3025,#3026,#3027));
#831=EDGE_LOOP('',(#3028,#3029));
#832=EDGE_LOOP('',(#3030,#3031));
#833=EDGE_LOOP('',(#3032,#3033,#3034,#3035));
#834=EDGE_LOOP('',(#3036,#3037,#3038,#3039,#3040,#3041,#3042,#3043,#3044));
#835=EDGE_LOOP('',(#3045,#3046,#3047));
#836=EDGE_LOOP('',(#3048,#3049,#3050,#3051,#3052,#3053));
#837=EDGE_LOOP('',(#3054,#3055,#3056,#3057,#3058,#3059,#3060,#3061));
#838=EDGE_LOOP('',(#3062,#3063,#3064,#3065,#3066));
#839=EDGE_LOOP('',(#3067,#3068,#3069,#3070));
#840=EDGE_LOOP('',(#3071,#3072,#3073,#3074,#3075,#3076));
#841=EDGE_LOOP('',(#3077,#3078,#3079,#3080,#3081,#3082));
#842=EDGE_LOOP('',(#3083,#3084,#3085,#3086));
#843=EDGE_LOOP('',(#3087,#3088,#3089,#3090));
#844=EDGE_LOOP('',(#3091,#3092,#3093,#3094,#3095,#3096));
#845=EDGE_LOOP('',(#3097,#3098,#3099,#3100));
#846=EDGE_LOOP('',(#3101));
#847=EDGE_LOOP('',(#3102,#3103,#3104,#3105));
#848=EDGE_LOOP('',(#3106,#3107,#3108,#3109));
#849=EDGE_LOOP('',(#3110,#3111,#3112,#3113));
#850=EDGE_LOOP('',(#3114,#3115,#3116,#3117));
#851=EDGE_LOOP('',(#3118,#3119,#3120,#3121));
#852=EDGE_LOOP('',(#3122,#3123,#3124,#3125));
#853=EDGE_LOOP('',(#3126,#3127,#3128,#3129,#3130,#3131));
#854=EDGE_LOOP('',(#3132,#3133,#3134,#3135,#3136,#3137));
#855=EDGE_LOOP('',(#3138));
#856=EDGE_LOOP('',(#3139));
#857=EDGE_LOOP('',(#3140,#3141,#3142,#3143));
#858=EDGE_LOOP('',(#3144,#3145,#3146,#3147));
#859=EDGE_LOOP('',(#3148,#3149,#3150,#3151));
#860=EDGE_LOOP('',(#3152));
#861=EDGE_LOOP('',(#3153));
#862=EDGE_LOOP('',(#3154,#3155,#3156,#3157));
#863=EDGE_LOOP('',(#3158,#3159,#3160,#3161));
#864=EDGE_LOOP('',(#3162,#3163,#3164,#3165));
#865=EDGE_LOOP('',(#3166,#3167,#3168,#3169));
#866=EDGE_LOOP('',(#3170,#3171,#3172,#3173));
#867=EDGE_LOOP('',(#3174,#3175,#3176,#3177));
#868=EDGE_LOOP('',(#3178,#3179,#3180,#3181));
#869=EDGE_LOOP('',(#3182,#3183,#3184,#3185));
#870=EDGE_LOOP('',(#3186));
#871=EDGE_LOOP('',(#3187));
#872=EDGE_LOOP('',(#3188));
#873=EDGE_LOOP('',(#3189));
#874=EDGE_LOOP('',(#3190));
#875=EDGE_LOOP('',(#3191,#3192,#3193,#3194));
#876=EDGE_LOOP('',(#3195,#3196,#3197,#3198));
#877=EDGE_LOOP('',(#3199));
#878=EDGE_LOOP('',(#3200));
#879=EDGE_LOOP('',(#3201));
#880=EDGE_LOOP('',(#3202));
#881=EDGE_LOOP('',(#3203));
#882=EDGE_LOOP('',(#3204,#3205,#3206,#3207));
#883=EDGE_LOOP('',(#3208,#3209,#3210,#3211));
#884=EDGE_LOOP('',(#3212,#3213,#3214,#3215));
#885=EDGE_LOOP('',(#3216,#3217,#3218,#3219));
#886=EDGE_LOOP('',(#3220,#3221,#3222,#3223));
#887=EDGE_LOOP('',(#3224,#3225,#3226,#3227));
#888=EDGE_LOOP('',(#3228,#3229,#3230,#3231));
#889=EDGE_LOOP('',(#3232,#3233,#3234,#3235));
#890=EDGE_LOOP('',(#3236,#3237,#3238,#3239));
#891=EDGE_LOOP('',(#3240,#3241,#3242,#3243));
#892=EDGE_LOOP('',(#3244,#3245,#3246,#3247));
#893=EDGE_LOOP('',(#3248,#3249,#3250,#3251));
#894=EDGE_LOOP('',(#3252));
#895=EDGE_LOOP('',(#3253,#3254,#3255,#3256,#3257,#3258,#3259,#3260));
#896=EDGE_LOOP('',(#3261));
#897=EDGE_LOOP('',(#3262));
#898=EDGE_LOOP('',(#3263,#3264,#3265,#3266,#3267,#3268,#3269,#3270));
#899=EDGE_LOOP('',(#3271));
#900=EDGE_LOOP('',(#3272));
#901=EDGE_LOOP('',(#3273,#3274,#3275,#3276));
#902=EDGE_LOOP('',(#3277,#3278,#3279,#3280));
#903=EDGE_LOOP('',(#3281));
#904=EDGE_LOOP('',(#3282));
#905=EDGE_LOOP('',(#3283,#3284,#3285,#3286));
#906=EDGE_LOOP('',(#3287,#3288,#3289,#3290));
#907=EDGE_LOOP('',(#3291,#3292,#3293,#3294));
#908=EDGE_LOOP('',(#3295));
#909=EDGE_LOOP('',(#3296));
#910=EDGE_LOOP('',(#3297,#3298,#3299,#3300));
#911=EDGE_LOOP('',(#3301,#3302,#3303,#3304));
#912=EDGE_LOOP('',(#3305,#3306,#3307,#3308));
#913=EDGE_LOOP('',(#3309));
#914=EDGE_LOOP('',(#3310,#3311,#3312,#3313));
#915=EDGE_LOOP('',(#3314,#3315,#3316,#3317));
#916=EDGE_LOOP('',(#3318,#3319,#3320,#3321));
#917=EDGE_LOOP('',(#3322,#3323,#3324,#3325));
#918=EDGE_LOOP('',(#3326,#3327,#3328,#3329));
#919=EDGE_LOOP('',(#3330,#3331,#3332,#3333));
#920=EDGE_LOOP('',(#3334,#3335,#3336,#3337,#3338,#3339));
#921=EDGE_LOOP('',(#3340,#3341,#3342,#3343,#3344,#3345));
#922=EDGE_LOOP('',(#3346,#3347,#3348,#3349,#3350,#3351,#3352,#3353,#3354));
#923=EDGE_LOOP('',(#3355,#3356,#3357,#3358,#3359,#3360,#3361,#3362,#3363));
#924=EDGE_LOOP('',(#3364,#3365,#3366,#3367));
#925=EDGE_LOOP('',(#3368,#3369,#3370,#3371));
#926=EDGE_LOOP('',(#3372,#3373,#3374,#3375));
#927=EDGE_LOOP('',(#3376,#3377,#3378,#3379));
#928=EDGE_LOOP('',(#3380,#3381,#3382,#3383));
#929=EDGE_LOOP('',(#3384,#3385,#3386,#3387));
#930=EDGE_LOOP('',(#3388,#3389,#3390,#3391));
#931=EDGE_LOOP('',(#3392));
#932=EDGE_LOOP('',(#3393));
#933=EDGE_LOOP('',(#3394));
#934=EDGE_LOOP('',(#3395));
#935=EDGE_LOOP('',(#3396,#3397,#3398,#3399));
#936=EDGE_LOOP('',(#3400,#3401,#3402,#3403));
#937=EDGE_LOOP('',(#3404));
#938=EDGE_LOOP('',(#3405));
#939=EDGE_LOOP('',(#3406,#3407,#3408,#3409));
#940=EDGE_LOOP('',(#3410));
#941=EDGE_LOOP('',(#3411));
#942=EDGE_LOOP('',(#3412));
#943=EDGE_LOOP('',(#3413,#3414,#3415,#3416));
#944=EDGE_LOOP('',(#3417,#3418,#3419,#3420));
#945=EDGE_LOOP('',(#3421,#3422,#3423,#3424));
#946=EDGE_LOOP('',(#3425));
#947=EDGE_LOOP('',(#3426));
#948=EDGE_LOOP('',(#3427,#3428,#3429,#3430));
#949=EDGE_LOOP('',(#3431,#3432,#3433,#3434));
#950=EDGE_LOOP('',(#3435,#3436,#3437,#3438));
#951=EDGE_LOOP('',(#3439));
#952=EDGE_LOOP('',(#3440,#3441,#3442,#3443));
#953=EDGE_LOOP('',(#3444,#3445,#3446,#3447));
#954=EDGE_LOOP('',(#3448,#3449,#3450,#3451));
#955=EDGE_LOOP('',(#3452,#3453,#3454,#3455));
#956=EDGE_LOOP('',(#3456,#3457,#3458,#3459));
#957=EDGE_LOOP('',(#3460,#3461,#3462,#3463));
#958=EDGE_LOOP('',(#3464,#3465,#3466,#3467,#3468,#3469));
#959=EDGE_LOOP('',(#3470,#3471,#3472,#3473,#3474,#3475));
#960=EDGE_LOOP('',(#3476,#3477,#3478,#3479,#3480,#3481,#3482,#3483,#3484));
#961=EDGE_LOOP('',(#3485,#3486,#3487,#3488,#3489,#3490,#3491,#3492,#3493));
#962=EDGE_LOOP('',(#3494,#3495,#3496,#3497));
#963=EDGE_LOOP('',(#3498,#3499,#3500,#3501));
#964=EDGE_LOOP('',(#3502,#3503,#3504,#3505));
#965=EDGE_LOOP('',(#3506,#3507,#3508,#3509));
#966=EDGE_LOOP('',(#3510,#3511,#3512,#3513));
#967=EDGE_LOOP('',(#3514,#3515,#3516,#3517));
#968=EDGE_LOOP('',(#3518,#3519,#3520,#3521));
#969=EDGE_LOOP('',(#3522));
#970=EDGE_LOOP('',(#3523));
#971=EDGE_LOOP('',(#3524));
#972=EDGE_LOOP('',(#3525));
#973=EDGE_LOOP('',(#3526,#3527,#3528,#3529));
#974=EDGE_LOOP('',(#3530,#3531,#3532,#3533));
#975=EDGE_LOOP('',(#3534));
#976=EDGE_LOOP('',(#3535,#3536,#3537,#3538));
#977=EDGE_LOOP('',(#3539,#3540,#3541,#3542));
#978=EDGE_LOOP('',(#3543));
#979=EDGE_LOOP('',(#3544,#3545,#3546,#3547));
#980=EDGE_LOOP('',(#3548,#3549,#3550,#3551));
#981=EDGE_LOOP('',(#3552,#3553,#3554,#3555));
#982=LINE('',#5469,#1340);
#983=LINE('',#5475,#1341);
#984=LINE('',#5480,#1342);
#985=LINE('',#5482,#1343);
#986=LINE('',#5484,#1344);
#987=LINE('',#5485,#1345);
#988=LINE('',#5488,#1346);
#989=LINE('',#5490,#1347);
#990=LINE('',#5491,#1348);
#991=LINE('',#5494,#1349);
#992=LINE('',#5496,#1350);
#993=LINE('',#5497,#1351);
#994=LINE('',#5499,#1352);
#995=LINE('',#5500,#1353);
#996=LINE('',#5507,#1354);
#997=LINE('',#5509,#1355);
#998=LINE('',#5511,#1356);
#999=LINE('',#5512,#1357);
#1000=LINE('',#5515,#1358);
#1001=LINE('',#5517,#1359);
#1002=LINE('',#5518,#1360);
#1003=LINE('',#5521,#1361);
#1004=LINE('',#5523,#1362);
#1005=LINE('',#5524,#1363);
#1006=LINE('',#5527,#1364);
#1007=LINE('',#5529,#1365);
#1008=LINE('',#5530,#1366);
#1009=LINE('',#5533,#1367);
#1010=LINE('',#5535,#1368);
#1011=LINE('',#5536,#1369);
#1012=LINE('',#5539,#1370);
#1013=LINE('',#5541,#1371);
#1014=LINE('',#5542,#1372);
#1015=LINE('',#5545,#1373);
#1016=LINE('',#5547,#1374);
#1017=LINE('',#5548,#1375);
#1018=LINE('',#5551,#1376);
#1019=LINE('',#5553,#1377);
#1020=LINE('',#5554,#1378);
#1021=LINE('',#5557,#1379);
#1022=LINE('',#5559,#1380);
#1023=LINE('',#5560,#1381);
#1024=LINE('',#5564,#1382);
#1025=LINE('',#5566,#1383);
#1026=LINE('',#5568,#1384);
#1027=LINE('',#5569,#1385);
#1028=LINE('',#5572,#1386);
#1029=LINE('',#5574,#1387);
#1030=LINE('',#5575,#1388);
#1031=LINE('',#5578,#1389);
#1032=LINE('',#5580,#1390);
#1033=LINE('',#5581,#1391);
#1034=LINE('',#5584,#1392);
#1035=LINE('',#5586,#1393);
#1036=LINE('',#5587,#1394);
#1037=LINE('',#5590,#1395);
#1038=LINE('',#5592,#1396);
#1039=LINE('',#5593,#1397);
#1040=LINE('',#5596,#1398);
#1041=LINE('',#5598,#1399);
#1042=LINE('',#5599,#1400);
#1043=LINE('',#5602,#1401);
#1044=LINE('',#5604,#1402);
#1045=LINE('',#5605,#1403);
#1046=LINE('',#5608,#1404);
#1047=LINE('',#5610,#1405);
#1048=LINE('',#5611,#1406);
#1049=LINE('',#5614,#1407);
#1050=LINE('',#5616,#1408);
#1051=LINE('',#5617,#1409);
#1052=LINE('',#5621,#1410);
#1053=LINE('',#5623,#1411);
#1054=LINE('',#5625,#1412);
#1055=LINE('',#5626,#1413);
#1056=LINE('',#5629,#1414);
#1057=LINE('',#5631,#1415);
#1058=LINE('',#5632,#1416);
#1059=LINE('',#5635,#1417);
#1060=LINE('',#5637,#1418);
#1061=LINE('',#5638,#1419);
#1062=LINE('',#5641,#1420);
#1063=LINE('',#5643,#1421);
#1064=LINE('',#5644,#1422);
#1065=LINE('',#5647,#1423);
#1066=LINE('',#5649,#1424);
#1067=LINE('',#5650,#1425);
#1068=LINE('',#5653,#1426);
#1069=LINE('',#5655,#1427);
#1070=LINE('',#5656,#1428);
#1071=LINE('',#5659,#1429);
#1072=LINE('',#5661,#1430);
#1073=LINE('',#5662,#1431);
#1074=LINE('',#5665,#1432);
#1075=LINE('',#5667,#1433);
#1076=LINE('',#5668,#1434);
#1077=LINE('',#5671,#1435);
#1078=LINE('',#5673,#1436);
#1079=LINE('',#5674,#1437);
#1080=LINE('',#5678,#1438);
#1081=LINE('',#5680,#1439);
#1082=LINE('',#5682,#1440);
#1083=LINE('',#5683,#1441);
#1084=LINE('',#5686,#1442);
#1085=LINE('',#5688,#1443);
#1086=LINE('',#5689,#1444);
#1087=LINE('',#5692,#1445);
#1088=LINE('',#5694,#1446);
#1089=LINE('',#5695,#1447);
#1090=LINE('',#5698,#1448);
#1091=LINE('',#5700,#1449);
#1092=LINE('',#5701,#1450);
#1093=LINE('',#5704,#1451);
#1094=LINE('',#5706,#1452);
#1095=LINE('',#5707,#1453);
#1096=LINE('',#5710,#1454);
#1097=LINE('',#5712,#1455);
#1098=LINE('',#5713,#1456);
#1099=LINE('',#5716,#1457);
#1100=LINE('',#5718,#1458);
#1101=LINE('',#5719,#1459);
#1102=LINE('',#5722,#1460);
#1103=LINE('',#5724,#1461);
#1104=LINE('',#5725,#1462);
#1105=LINE('',#5728,#1463);
#1106=LINE('',#5730,#1464);
#1107=LINE('',#5731,#1465);
#1108=LINE('',#5736,#1466);
#1109=LINE('',#5740,#1467);
#1110=LINE('',#5742,#1468);
#1111=LINE('',#5743,#1469);
#1112=LINE('',#5746,#1470);
#1113=LINE('',#5748,#1471);
#1114=LINE('',#5749,#1472);
#1115=LINE('',#5751,#1473);
#1116=LINE('',#5752,#1474);
#1117=LINE('',#5755,#1475);
#1118=LINE('',#5757,#1476);
#1119=LINE('',#5758,#1477);
#1120=LINE('',#5760,#1478);
#1121=LINE('',#5761,#1479);
#1122=LINE('',#5764,#1480);
#1123=LINE('',#5766,#1481);
#1124=LINE('',#5767,#1482);
#1125=LINE('',#5769,#1483);
#1126=LINE('',#5770,#1484);
#1127=LINE('',#5772,#1485);
#1128=LINE('',#5773,#1486);
#1129=LINE('',#5781,#1487);
#1130=LINE('',#5787,#1488);
#1131=LINE('',#5793,#1489);
#1132=LINE('',#5799,#1490);
#1133=LINE('',#5804,#1491);
#1134=LINE('',#5806,#1492);
#1135=LINE('',#5808,#1493);
#1136=LINE('',#5809,#1494);
#1137=LINE('',#5813,#1495);
#1138=LINE('',#5814,#1496);
#1139=LINE('',#5815,#1497);
#1140=LINE('',#5818,#1498);
#1141=LINE('',#5820,#1499);
#1142=LINE('',#5822,#1500);
#1143=LINE('',#5824,#1501);
#1144=LINE('',#5826,#1502);
#1145=LINE('',#5828,#1503);
#1146=LINE('',#5829,#1504);
#1147=LINE('',#5833,#1505);
#1148=LINE('',#5837,#1506);
#1149=LINE('',#5840,#1507);
#1150=LINE('',#5842,#1508);
#1151=LINE('',#5844,#1509);
#1152=LINE('',#5846,#1510);
#1153=LINE('',#5847,#1511);
#1154=LINE('',#5854,#1512);
#1155=LINE('',#5855,#1513);
#1156=LINE('',#5858,#1514);
#1157=LINE('',#5859,#1515);
#1158=LINE('',#5861,#1516);
#1159=LINE('',#5878,#1517);
#1160=LINE('',#5948,#1518);
#1161=LINE('',#5952,#1519);
#1162=LINE('',#5959,#1520);
#1163=LINE('',#5960,#1521);
#1164=LINE('',#5964,#1522);
#1165=LINE('',#5971,#1523);
#1166=LINE('',#5977,#1524);
#1167=LINE('',#6044,#1525);
#1168=LINE('',#6047,#1526);
#1169=LINE('',#6049,#1527);
#1170=LINE('',#6050,#1528);
#1171=LINE('',#6054,#1529);
#1172=LINE('',#6061,#1530);
#1173=LINE('',#6063,#1531);
#1174=LINE('',#6065,#1532);
#1175=LINE('',#6067,#1533);
#1176=LINE('',#6070,#1534);
#1177=LINE('',#6075,#1535);
#1178=LINE('',#6084,#1536);
#1179=LINE('',#6085,#1537);
#1180=LINE('',#6088,#1538);
#1181=LINE('',#6089,#1539);
#1182=LINE('',#6092,#1540);
#1183=LINE('',#6094,#1541);
#1184=LINE('',#6095,#1542);
#1185=LINE('',#6098,#1543);
#1186=LINE('',#6100,#1544);
#1187=LINE('',#6101,#1545);
#1188=LINE('',#6104,#1546);
#1189=LINE('',#6105,#1547);
#1190=LINE('',#6108,#1548);
#1191=LINE('',#6109,#1549);
#1192=LINE('',#6111,#1550);
#1193=LINE('',#6117,#1551);
#1194=LINE('',#6119,#1552);
#1195=LINE('',#6121,#1553);
#1196=LINE('',#6122,#1554);
#1197=LINE('',#6125,#1555);
#1198=LINE('',#6127,#1556);
#1199=LINE('',#6128,#1557);
#1200=LINE('',#6131,#1558);
#1201=LINE('',#6133,#1559);
#1202=LINE('',#6134,#1560);
#1203=LINE('',#6137,#1561);
#1204=LINE('',#6139,#1562);
#1205=LINE('',#6140,#1563);
#1206=LINE('',#6143,#1564);
#1207=LINE('',#6145,#1565);
#1208=LINE('',#6146,#1566);
#1209=LINE('',#6148,#1567);
#1210=LINE('',#6149,#1568);
#1211=LINE('',#6161,#1569);
#1212=LINE('',#6165,#1570);
#1213=LINE('',#6169,#1571);
#1214=LINE('',#6176,#1572);
#1215=LINE('',#6178,#1573);
#1216=LINE('',#6185,#1574);
#1217=LINE('',#6191,#1575);
#1218=LINE('',#6197,#1576);
#1219=LINE('',#6203,#1577);
#1220=LINE('',#6209,#1578);
#1221=LINE('',#6214,#1579);
#1222=LINE('',#6216,#1580);
#1223=LINE('',#6218,#1581);
#1224=LINE('',#6219,#1582);
#1225=LINE('',#6222,#1583);
#1226=LINE('',#6224,#1584);
#1227=LINE('',#6225,#1585);
#1228=LINE('',#6228,#1586);
#1229=LINE('',#6230,#1587);
#1230=LINE('',#6231,#1588);
#1231=LINE('',#6233,#1589);
#1232=LINE('',#6234,#1590);
#1233=LINE('',#6242,#1591);
#1234=LINE('',#6248,#1592);
#1235=LINE('',#6254,#1593);
#1236=LINE('',#6259,#1594);
#1237=LINE('',#6261,#1595);
#1238=LINE('',#6263,#1596);
#1239=LINE('',#6264,#1597);
#1240=LINE('',#6268,#1598);
#1241=LINE('',#6270,#1599);
#1242=LINE('',#6272,#1600);
#1243=LINE('',#6273,#1601);
#1244=LINE('',#6276,#1602);
#1245=LINE('',#6278,#1603);
#1246=LINE('',#6279,#1604);
#1247=LINE('',#6282,#1605);
#1248=LINE('',#6284,#1606);
#1249=LINE('',#6285,#1607);
#1250=LINE('',#6287,#1608);
#1251=LINE('',#6288,#1609);
#1252=LINE('',#6291,#1610);
#1253=LINE('',#6294,#1611);
#1254=LINE('',#6297,#1612);
#1255=LINE('',#6298,#1613);
#1256=LINE('',#6301,#1614);
#1257=LINE('',#6302,#1615);
#1258=LINE('',#6313,#1616);
#1259=LINE('',#6317,#1617);
#1260=LINE('',#6321,#1618);
#1261=LINE('',#6328,#1619);
#1262=LINE('',#6332,#1620);
#1263=LINE('',#6336,#1621);
#1264=LINE('',#6341,#1622);
#1265=LINE('',#6343,#1623);
#1266=LINE('',#6345,#1624);
#1267=LINE('',#6346,#1625);
#1268=LINE('',#6349,#1626);
#1269=LINE('',#6351,#1627);
#1270=LINE('',#6352,#1628);
#1271=LINE('',#6355,#1629);
#1272=LINE('',#6357,#1630);
#1273=LINE('',#6358,#1631);
#1274=LINE('',#6361,#1632);
#1275=LINE('',#6363,#1633);
#1276=LINE('',#6364,#1634);
#1277=LINE('',#6367,#1635);
#1278=LINE('',#6369,#1636);
#1279=LINE('',#6370,#1637);
#1280=LINE('',#6372,#1638);
#1281=LINE('',#6373,#1639);
#1282=LINE('',#6388,#1640);
#1283=LINE('',#6409,#1641);
#1284=LINE('',#6434,#1642);
#1285=LINE('',#6435,#1643);
#1286=LINE('',#6437,#1644);
#1287=LINE('',#6439,#1645);
#1288=LINE('',#6444,#1646);
#1289=LINE('',#6447,#1647);
#1290=LINE('',#6449,#1648);
#1291=LINE('',#6458,#1649);
#1292=LINE('',#6462,#1650);
#1293=LINE('',#6469,#1651);
#1294=LINE('',#6510,#1652);
#1295=LINE('',#6514,#1653);
#1296=LINE('',#6518,#1654);
#1297=LINE('',#6525,#1655);
#1298=LINE('',#6529,#1656);
#1299=LINE('',#6533,#1657);
#1300=LINE('',#6538,#1658);
#1301=LINE('',#6540,#1659);
#1302=LINE('',#6542,#1660);
#1303=LINE('',#6543,#1661);
#1304=LINE('',#6546,#1662);
#1305=LINE('',#6548,#1663);
#1306=LINE('',#6549,#1664);
#1307=LINE('',#6552,#1665);
#1308=LINE('',#6554,#1666);
#1309=LINE('',#6555,#1667);
#1310=LINE('',#6558,#1668);
#1311=LINE('',#6560,#1669);
#1312=LINE('',#6561,#1670);
#1313=LINE('',#6564,#1671);
#1314=LINE('',#6566,#1672);
#1315=LINE('',#6567,#1673);
#1316=LINE('',#6569,#1674);
#1317=LINE('',#6570,#1675);
#1318=LINE('',#6585,#1676);
#1319=LINE('',#6606,#1677);
#1320=LINE('',#6631,#1678);
#1321=LINE('',#6632,#1679);
#1322=LINE('',#6634,#1680);
#1323=LINE('',#6636,#1681);
#1324=LINE('',#6641,#1682);
#1325=LINE('',#6644,#1683);
#1326=LINE('',#6646,#1684);
#1327=LINE('',#6670,#1685);
#1328=LINE('',#6675,#1686);
#1329=LINE('',#6677,#1687);
#1330=LINE('',#6679,#1688);
#1331=LINE('',#6680,#1689);
#1332=LINE('',#6683,#1690);
#1333=LINE('',#6685,#1691);
#1334=LINE('',#6686,#1692);
#1335=LINE('',#6689,#1693);
#1336=LINE('',#6691,#1694);
#1337=LINE('',#6692,#1695);
#1338=LINE('',#6694,#1696);
#1339=LINE('',#6695,#1697);
#1340=VECTOR('',#4374,0.274999999999999);
#1341=VECTOR('',#4381,0.274999999999999);
#1342=VECTOR('',#4386,1.);
#1343=VECTOR('',#4387,1.);
#1344=VECTOR('',#4388,1.);
#1345=VECTOR('',#4389,1.);
#1346=VECTOR('',#4392,1.);
#1347=VECTOR('',#4393,1.);
#1348=VECTOR('',#4394,1.);
#1349=VECTOR('',#4397,1.);
#1350=VECTOR('',#4398,1.);
#1351=VECTOR('',#4399,1.);
#1352=VECTOR('',#4402,1.);
#1353=VECTOR('',#4403,1.);
#1354=VECTOR('',#4412,1.);
#1355=VECTOR('',#4413,1.);
#1356=VECTOR('',#4414,1.);
#1357=VECTOR('',#4415,1.);
#1358=VECTOR('',#4418,1.);
#1359=VECTOR('',#4419,1.);
#1360=VECTOR('',#4420,1.);
#1361=VECTOR('',#4423,1.);
#1362=VECTOR('',#4424,1.);
#1363=VECTOR('',#4425,1.);
#1364=VECTOR('',#4428,1.);
#1365=VECTOR('',#4429,1.);
#1366=VECTOR('',#4430,1.);
#1367=VECTOR('',#4433,1.);
#1368=VECTOR('',#4434,1.);
#1369=VECTOR('',#4435,1.);
#1370=VECTOR('',#4438,1.);
#1371=VECTOR('',#4439,1.);
#1372=VECTOR('',#4440,1.);
#1373=VECTOR('',#4443,1.);
#1374=VECTOR('',#4444,1.);
#1375=VECTOR('',#4445,1.);
#1376=VECTOR('',#4448,1.);
#1377=VECTOR('',#4449,1.);
#1378=VECTOR('',#4450,1.);
#1379=VECTOR('',#4453,1.);
#1380=VECTOR('',#4454,1.);
#1381=VECTOR('',#4455,1.);
#1382=VECTOR('',#4458,1.);
#1383=VECTOR('',#4459,1.);
#1384=VECTOR('',#4460,1.);
#1385=VECTOR('',#4461,1.);
#1386=VECTOR('',#4464,1.);
#1387=VECTOR('',#4465,1.);
#1388=VECTOR('',#4466,1.);
#1389=VECTOR('',#4469,1.);
#1390=VECTOR('',#4470,1.);
#1391=VECTOR('',#4471,1.);
#1392=VECTOR('',#4474,1.);
#1393=VECTOR('',#4475,1.);
#1394=VECTOR('',#4476,1.);
#1395=VECTOR('',#4479,1.);
#1396=VECTOR('',#4480,1.);
#1397=VECTOR('',#4481,1.);
#1398=VECTOR('',#4484,1.);
#1399=VECTOR('',#4485,1.);
#1400=VECTOR('',#4486,1.);
#1401=VECTOR('',#4489,1.);
#1402=VECTOR('',#4490,1.);
#1403=VECTOR('',#4491,1.);
#1404=VECTOR('',#4494,1.);
#1405=VECTOR('',#4495,1.);
#1406=VECTOR('',#4496,1.);
#1407=VECTOR('',#4499,1.);
#1408=VECTOR('',#4500,1.);
#1409=VECTOR('',#4501,1.);
#1410=VECTOR('',#4504,1.);
#1411=VECTOR('',#4505,1.);
#1412=VECTOR('',#4506,1.);
#1413=VECTOR('',#4507,1.);
#1414=VECTOR('',#4510,1.);
#1415=VECTOR('',#4511,1.);
#1416=VECTOR('',#4512,1.);
#1417=VECTOR('',#4515,1.);
#1418=VECTOR('',#4516,1.);
#1419=VECTOR('',#4517,1.);
#1420=VECTOR('',#4520,1.);
#1421=VECTOR('',#4521,1.);
#1422=VECTOR('',#4522,1.);
#1423=VECTOR('',#4525,1.);
#1424=VECTOR('',#4526,1.);
#1425=VECTOR('',#4527,1.);
#1426=VECTOR('',#4530,1.);
#1427=VECTOR('',#4531,1.);
#1428=VECTOR('',#4532,1.);
#1429=VECTOR('',#4535,1.);
#1430=VECTOR('',#4536,1.);
#1431=VECTOR('',#4537,1.);
#1432=VECTOR('',#4540,1.);
#1433=VECTOR('',#4541,1.);
#1434=VECTOR('',#4542,1.);
#1435=VECTOR('',#4545,1.);
#1436=VECTOR('',#4546,1.);
#1437=VECTOR('',#4547,1.);
#1438=VECTOR('',#4550,1.);
#1439=VECTOR('',#4551,1.);
#1440=VECTOR('',#4552,1.);
#1441=VECTOR('',#4553,1.);
#1442=VECTOR('',#4556,1.);
#1443=VECTOR('',#4557,1.);
#1444=VECTOR('',#4558,1.);
#1445=VECTOR('',#4561,1.);
#1446=VECTOR('',#4562,1.);
#1447=VECTOR('',#4563,1.);
#1448=VECTOR('',#4566,1.);
#1449=VECTOR('',#4567,1.);
#1450=VECTOR('',#4568,1.);
#1451=VECTOR('',#4571,1.);
#1452=VECTOR('',#4572,1.);
#1453=VECTOR('',#4573,1.);
#1454=VECTOR('',#4576,1.);
#1455=VECTOR('',#4577,1.);
#1456=VECTOR('',#4578,1.);
#1457=VECTOR('',#4581,1.);
#1458=VECTOR('',#4582,1.);
#1459=VECTOR('',#4583,1.);
#1460=VECTOR('',#4586,1.);
#1461=VECTOR('',#4587,1.);
#1462=VECTOR('',#4588,1.);
#1463=VECTOR('',#4591,1.);
#1464=VECTOR('',#4592,1.);
#1465=VECTOR('',#4593,1.);
#1466=VECTOR('',#4598,0.21);
#1467=VECTOR('',#4603,1.);
#1468=VECTOR('',#4604,1.);
#1469=VECTOR('',#4605,1.);
#1470=VECTOR('',#4608,1.);
#1471=VECTOR('',#4609,1.);
#1472=VECTOR('',#4610,1.);
#1473=VECTOR('',#4613,1.);
#1474=VECTOR('',#4614,1.);
#1475=VECTOR('',#4617,1.);
#1476=VECTOR('',#4618,1.);
#1477=VECTOR('',#4619,1.);
#1478=VECTOR('',#4622,1.);
#1479=VECTOR('',#4623,1.);
#1480=VECTOR('',#4626,1.);
#1481=VECTOR('',#4627,1.);
#1482=VECTOR('',#4628,1.);
#1483=VECTOR('',#4631,1.);
#1484=VECTOR('',#4632,1.);
#1485=VECTOR('',#4635,1.);
#1486=VECTOR('',#4636,1.);
#1487=VECTOR('',#4647,0.275);
#1488=VECTOR('',#4654,0.275);
#1489=VECTOR('',#4661,0.31);
#1490=VECTOR('',#4668,0.31);
#1491=VECTOR('',#4673,1.);
#1492=VECTOR('',#4674,1.);
#1493=VECTOR('',#4675,1.);
#1494=VECTOR('',#4676,1.);
#1495=VECTOR('',#4679,1.);
#1496=VECTOR('',#4680,1.);
#1497=VECTOR('',#4681,1.);
#1498=VECTOR('',#4684,1.);
#1499=VECTOR('',#4685,1.);
#1500=VECTOR('',#4686,1.);
#1501=VECTOR('',#4687,1.);
#1502=VECTOR('',#4688,1.);
#1503=VECTOR('',#4689,1.);
#1504=VECTOR('',#4690,1.);
#1505=VECTOR('',#4693,1.);
#1506=VECTOR('',#4700,1.);
#1507=VECTOR('',#4703,1.);
#1508=VECTOR('',#4704,1.);
#1509=VECTOR('',#4705,1.);
#1510=VECTOR('',#4706,1.);
#1511=VECTOR('',#4707,1.);
#1512=VECTOR('',#4718,1.);
#1513=VECTOR('',#4719,1.);
#1514=VECTOR('',#4722,1.);
#1515=VECTOR('',#4723,1.);
#1516=VECTOR('',#4726,1.);
#1517=VECTOR('',#4733,0.08);
#1518=VECTOR('',#4742,0.475);
#1519=VECTOR('',#4747,0.5);
#1520=VECTOR('',#4756,0.3);
#1521=VECTOR('',#4757,0.3);
#1522=VECTOR('',#4762,0.255);
#1523=VECTOR('',#4771,0.32);
#1524=VECTOR('',#4778,0.6);
#1525=VECTOR('',#4797,1.);
#1526=VECTOR('',#4800,1.);
#1527=VECTOR('',#4801,1.);
#1528=VECTOR('',#4802,1.);
#1529=VECTOR('',#4807,0.08);
#1530=VECTOR('',#4816,1.);
#1531=VECTOR('',#4817,1.);
#1532=VECTOR('',#4818,1.);
#1533=VECTOR('',#4819,1.);
#1534=VECTOR('',#4822,1.);
#1535=VECTOR('',#4827,0.21);
#1536=VECTOR('',#4838,1.);
#1537=VECTOR('',#4839,1.);
#1538=VECTOR('',#4842,1.);
#1539=VECTOR('',#4843,1.);
#1540=VECTOR('',#4846,1.);
#1541=VECTOR('',#4847,1.);
#1542=VECTOR('',#4848,1.);
#1543=VECTOR('',#4851,1.);
#1544=VECTOR('',#4852,1.);
#1545=VECTOR('',#4853,1.);
#1546=VECTOR('',#4856,1.);
#1547=VECTOR('',#4857,1.);
#1548=VECTOR('',#4860,1.);
#1549=VECTOR('',#4861,1.);
#1550=VECTOR('',#4864,1.);
#1551=VECTOR('',#4871,1.);
#1552=VECTOR('',#4872,1.);
#1553=VECTOR('',#4873,1.);
#1554=VECTOR('',#4874,1.);
#1555=VECTOR('',#4877,1.);
#1556=VECTOR('',#4878,1.);
#1557=VECTOR('',#4879,1.);
#1558=VECTOR('',#4882,1.);
#1559=VECTOR('',#4883,1.);
#1560=VECTOR('',#4884,1.);
#1561=VECTOR('',#4887,1.);
#1562=VECTOR('',#4888,1.);
#1563=VECTOR('',#4889,1.);
#1564=VECTOR('',#4892,1.);
#1565=VECTOR('',#4893,1.);
#1566=VECTOR('',#4894,1.);
#1567=VECTOR('',#4897,1.);
#1568=VECTOR('',#4898,1.);
#1569=VECTOR('',#4915,0.4);
#1570=VECTOR('',#4920,0.425);
#1571=VECTOR('',#4925,0.41);
#1572=VECTOR('',#4934,0.26);
#1573=VECTOR('',#4937,0.25);
#1574=VECTOR('',#4946,0.274999999999999);
#1575=VECTOR('',#4953,0.225);
#1576=VECTOR('',#4960,0.225);
#1577=VECTOR('',#4967,0.225);
#1578=VECTOR('',#4974,0.225);
#1579=VECTOR('',#4979,1.);
#1580=VECTOR('',#4980,1.);
#1581=VECTOR('',#4981,1.);
#1582=VECTOR('',#4982,1.);
#1583=VECTOR('',#4985,1.);
#1584=VECTOR('',#4986,1.);
#1585=VECTOR('',#4987,1.);
#1586=VECTOR('',#4990,1.);
#1587=VECTOR('',#4991,1.);
#1588=VECTOR('',#4992,1.);
#1589=VECTOR('',#4995,1.);
#1590=VECTOR('',#4996,1.);
#1591=VECTOR('',#5007,0.225);
#1592=VECTOR('',#5014,0.225);
#1593=VECTOR('',#5021,0.31);
#1594=VECTOR('',#5026,1.);
#1595=VECTOR('',#5027,1.);
#1596=VECTOR('',#5028,1.);
#1597=VECTOR('',#5029,1.);
#1598=VECTOR('',#5032,1.);
#1599=VECTOR('',#5033,1.);
#1600=VECTOR('',#5034,1.);
#1601=VECTOR('',#5035,1.);
#1602=VECTOR('',#5038,1.);
#1603=VECTOR('',#5039,1.);
#1604=VECTOR('',#5040,1.);
#1605=VECTOR('',#5043,1.);
#1606=VECTOR('',#5044,1.);
#1607=VECTOR('',#5045,1.);
#1608=VECTOR('',#5048,1.);
#1609=VECTOR('',#5049,1.);
#1610=VECTOR('',#5052,1.);
#1611=VECTOR('',#5055,1.);
#1612=VECTOR('',#5058,1.);
#1613=VECTOR('',#5059,1.);
#1614=VECTOR('',#5062,1.);
#1615=VECTOR('',#5063,1.);
#1616=VECTOR('',#5080,0.325);
#1617=VECTOR('',#5085,0.35);
#1618=VECTOR('',#5090,0.335);
#1619=VECTOR('',#5099,0.21);
#1620=VECTOR('',#5104,0.2);
#1621=VECTOR('',#5109,0.18);
#1622=VECTOR('',#5114,1.);
#1623=VECTOR('',#5115,1.);
#1624=VECTOR('',#5116,1.);
#1625=VECTOR('',#5117,1.);
#1626=VECTOR('',#5120,1.);
#1627=VECTOR('',#5121,1.);
#1628=VECTOR('',#5122,1.);
#1629=VECTOR('',#5125,1.);
#1630=VECTOR('',#5126,1.);
#1631=VECTOR('',#5127,1.);
#1632=VECTOR('',#5130,1.);
#1633=VECTOR('',#5131,1.);
#1634=VECTOR('',#5132,1.);
#1635=VECTOR('',#5135,1.);
#1636=VECTOR('',#5136,1.);
#1637=VECTOR('',#5137,1.);
#1638=VECTOR('',#5140,1.);
#1639=VECTOR('',#5141,1.);
#1640=VECTOR('',#5150,0.418322594216369);
#1641=VECTOR('',#5157,0.418322594216369);
#1642=VECTOR('',#5160,1.);
#1643=VECTOR('',#5161,1.);
#1644=VECTOR('',#5164,1.);
#1645=VECTOR('',#5167,1.);
#1646=VECTOR('',#5172,0.2);
#1647=VECTOR('',#5177,1.);
#1648=VECTOR('',#5180,1.);
#1649=VECTOR('',#5193,0.275);
#1650=VECTOR('',#5198,0.265);
#1651=VECTOR('',#5207,0.5);
#1652=VECTOR('',#5284,0.4);
#1653=VECTOR('',#5289,0.425);
#1654=VECTOR('',#5294,0.41);
#1655=VECTOR('',#5303,0.26);
#1656=VECTOR('',#5308,0.25);
#1657=VECTOR('',#5313,0.225);
#1658=VECTOR('',#5318,1.);
#1659=VECTOR('',#5319,1.);
#1660=VECTOR('',#5320,1.);
#1661=VECTOR('',#5321,1.);
#1662=VECTOR('',#5324,1.);
#1663=VECTOR('',#5325,1.);
#1664=VECTOR('',#5326,1.);
#1665=VECTOR('',#5329,1.);
#1666=VECTOR('',#5330,1.);
#1667=VECTOR('',#5331,1.);
#1668=VECTOR('',#5334,1.);
#1669=VECTOR('',#5335,1.);
#1670=VECTOR('',#5336,1.);
#1671=VECTOR('',#5339,1.);
#1672=VECTOR('',#5340,1.);
#1673=VECTOR('',#5341,1.);
#1674=VECTOR('',#5344,1.);
#1675=VECTOR('',#5345,1.);
#1676=VECTOR('',#5354,0.47094010767585);
#1677=VECTOR('',#5361,0.47094010767585);
#1678=VECTOR('',#5364,1.);
#1679=VECTOR('',#5365,1.);
#1680=VECTOR('',#5368,1.);
#1681=VECTOR('',#5371,1.);
#1682=VECTOR('',#5376,0.25);
#1683=VECTOR('',#5381,1.);
#1684=VECTOR('',#5384,1.);
#1685=VECTOR('',#5427,0.274999999999999);
#1686=VECTOR('',#5432,1.);
#1687=VECTOR('',#5433,1.);
#1688=VECTOR('',#5434,1.);
#1689=VECTOR('',#5435,1.);
#1690=VECTOR('',#5438,1.);
#1691=VECTOR('',#5439,1.);
#1692=VECTOR('',#5440,1.);
#1693=VECTOR('',#5443,1.);
#1694=VECTOR('',#5444,1.);
#1695=VECTOR('',#5445,1.);
#1696=VECTOR('',#5448,1.);
#1697=VECTOR('',#5449,1.);
#1698=CIRCLE('',#3998,0.274999999999999);
#1699=CIRCLE('',#3999,0.274999999999999);
#1700=CIRCLE('',#4001,0.274999999999999);
#1701=CIRCLE('',#4002,0.274999999999999);
#1702=CIRCLE('',#4047,0.21);
#1703=CIRCLE('',#4048,0.21);
#1704=CIRCLE('',#4061,0.275);
#1705=CIRCLE('',#4062,0.275);
#1706=CIRCLE('',#4064,0.275);
#1707=CIRCLE('',#4065,0.275);
#1708=CIRCLE('',#4067,0.31);
#1709=CIRCLE('',#4068,0.31);
#1710=CIRCLE('',#4070,0.31);
#1711=CIRCLE('',#4071,0.31);
#1712=CIRCLE('',#4076,0.6);
#1713=CIRCLE('',#4077,0.6);
#1714=CIRCLE('',#4081,0.6);
#1715=CIRCLE('',#4083,0.6);
#1716=CIRCLE('',#4091,0.45);
#1717=CIRCLE('',#4093,0.5);
#1718=CIRCLE('',#4095,0.5);
#1719=CIRCLE('',#4097,0.3);
#1720=CIRCLE('',#4099,0.3);
#1721=CIRCLE('',#4101,0.21);
#1722=CIRCLE('',#4105,0.32);
#1723=CIRCLE('',#4106,0.32);
#1724=CIRCLE('',#4108,0.6);
#1725=CIRCLE('',#4109,0.6);
#1726=CIRCLE('',#4114,0.08);
#1727=CIRCLE('',#4115,0.04);
#1728=CIRCLE('',#4117,0.08);
#1729=CIRCLE('',#4120,0.08);
#1730=CIRCLE('',#4121,0.08);
#1731=CIRCLE('',#4127,0.2117);
#1732=CIRCLE('',#4128,0.2117);
#1733=CIRCLE('',#4129,0.2117);
#1734=CIRCLE('',#4131,0.2117);
#1735=CIRCLE('',#4150,0.24505);
#1736=CIRCLE('',#4152,0.375);
#1737=CIRCLE('',#4154,0.425);
#1738=CIRCLE('',#4156,0.425);
#1739=CIRCLE('',#4158,0.395);
#1740=CIRCLE('',#4160,0.27);
#1741=CIRCLE('',#4162,0.24505);
#1742=CIRCLE('',#4167,0.274999999999999);
#1743=CIRCLE('',#4168,0.274999999999999);
#1744=CIRCLE('',#4170,0.225);
#1745=CIRCLE('',#4171,0.225);
#1746=CIRCLE('',#4173,0.225);
#1747=CIRCLE('',#4174,0.225);
#1748=CIRCLE('',#4176,0.225);
#1749=CIRCLE('',#4177,0.225);
#1750=CIRCLE('',#4179,0.225);
#1751=CIRCLE('',#4180,0.225);
#1752=CIRCLE('',#4189,0.225);
#1753=CIRCLE('',#4190,0.225);
#1754=CIRCLE('',#4192,0.225);
#1755=CIRCLE('',#4193,0.225);
#1756=CIRCLE('',#4195,0.31);
#1757=CIRCLE('',#4196,0.31);
#1758=CIRCLE('',#4203,0.6);
#1759=CIRCLE('',#4207,0.6);
#1760=CIRCLE('',#4211,0.3);
#1761=CIRCLE('',#4213,0.35);
#1762=CIRCLE('',#4215,0.35);
#1763=CIRCLE('',#4217,0.32);
#1764=CIRCLE('',#4219,0.22);
#1765=CIRCLE('',#4221,0.1954);
#1766=CIRCLE('',#4223,0.1954);
#1767=CIRCLE('',#4225,0.16);
#1768=CIRCLE('',#4237,0.3325);
#1769=CIRCLE('',#4239,0.3325);
#1770=CIRCLE('',#4244,0.1666);
#1771=CIRCLE('',#4245,0.1666);
#1772=CIRCLE('',#4253,0.285);
#1773=CIRCLE('',#4254,0.265);
#1774=CIRCLE('',#4256,0.265);
#1775=CIRCLE('',#4258,0.5);
#1776=CIRCLE('',#4260,0.5);
#1777=CIRCLE('',#4295,0.375);
#1778=CIRCLE('',#4297,0.425);
#1779=CIRCLE('',#4299,0.425);
#1780=CIRCLE('',#4301,0.395);
#1781=CIRCLE('',#4303,0.27);
#1782=CIRCLE('',#4305,0.24505);
#1783=CIRCLE('',#4307,0.24505);
#1784=CIRCLE('',#4309,0.2);
#1785=CIRCLE('',#4321,0.38);
#1786=CIRCLE('',#4323,0.38);
#1787=CIRCLE('',#4328,0.2117);
#1788=CIRCLE('',#4329,0.2117);
#1789=CIRCLE('',#4352,0.274999999999999);
#1790=CIRCLE('',#4353,0.274999999999999);
#1791=VERTEX_POINT('',#5466);
#1792=VERTEX_POINT('',#5468);
#1793=VERTEX_POINT('',#5472);
#1794=VERTEX_POINT('',#5474);
#1795=VERTEX_POINT('',#5478);
#1796=VERTEX_POINT('',#5479);
#1797=VERTEX_POINT('',#5481);
#1798=VERTEX_POINT('',#5483);
#1799=VERTEX_POINT('',#5487);
#1800=VERTEX_POINT('',#5489);
#1801=VERTEX_POINT('',#5493);
#1802=VERTEX_POINT('',#5495);
#1803=VERTEX_POINT('',#5505);
#1804=VERTEX_POINT('',#5506);
#1805=VERTEX_POINT('',#5508);
#1806=VERTEX_POINT('',#5510);
#1807=VERTEX_POINT('',#5514);
#1808=VERTEX_POINT('',#5516);
#1809=VERTEX_POINT('',#5520);
#1810=VERTEX_POINT('',#5522);
#1811=VERTEX_POINT('',#5526);
#1812=VERTEX_POINT('',#5528);
#1813=VERTEX_POINT('',#5532);
#1814=VERTEX_POINT('',#5534);
#1815=VERTEX_POINT('',#5538);
#1816=VERTEX_POINT('',#5540);
#1817=VERTEX_POINT('',#5544);
#1818=VERTEX_POINT('',#5546);
#1819=VERTEX_POINT('',#5550);
#1820=VERTEX_POINT('',#5552);
#1821=VERTEX_POINT('',#5556);
#1822=VERTEX_POINT('',#5558);
#1823=VERTEX_POINT('',#5562);
#1824=VERTEX_POINT('',#5563);
#1825=VERTEX_POINT('',#5565);
#1826=VERTEX_POINT('',#5567);
#1827=VERTEX_POINT('',#5571);
#1828=VERTEX_POINT('',#5573);
#1829=VERTEX_POINT('',#5577);
#1830=VERTEX_POINT('',#5579);
#1831=VERTEX_POINT('',#5583);
#1832=VERTEX_POINT('',#5585);
#1833=VERTEX_POINT('',#5589);
#1834=VERTEX_POINT('',#5591);
#1835=VERTEX_POINT('',#5595);
#1836=VERTEX_POINT('',#5597);
#1837=VERTEX_POINT('',#5601);
#1838=VERTEX_POINT('',#5603);
#1839=VERTEX_POINT('',#5607);
#1840=VERTEX_POINT('',#5609);
#1841=VERTEX_POINT('',#5613);
#1842=VERTEX_POINT('',#5615);
#1843=VERTEX_POINT('',#5619);
#1844=VERTEX_POINT('',#5620);
#1845=VERTEX_POINT('',#5622);
#1846=VERTEX_POINT('',#5624);
#1847=VERTEX_POINT('',#5628);
#1848=VERTEX_POINT('',#5630);
#1849=VERTEX_POINT('',#5634);
#1850=VERTEX_POINT('',#5636);
#1851=VERTEX_POINT('',#5640);
#1852=VERTEX_POINT('',#5642);
#1853=VERTEX_POINT('',#5646);
#1854=VERTEX_POINT('',#5648);
#1855=VERTEX_POINT('',#5652);
#1856=VERTEX_POINT('',#5654);
#1857=VERTEX_POINT('',#5658);
#1858=VERTEX_POINT('',#5660);
#1859=VERTEX_POINT('',#5664);
#1860=VERTEX_POINT('',#5666);
#1861=VERTEX_POINT('',#5670);
#1862=VERTEX_POINT('',#5672);
#1863=VERTEX_POINT('',#5676);
#1864=VERTEX_POINT('',#5677);
#1865=VERTEX_POINT('',#5679);
#1866=VERTEX_POINT('',#5681);
#1867=VERTEX_POINT('',#5685);
#1868=VERTEX_POINT('',#5687);
#1869=VERTEX_POINT('',#5691);
#1870=VERTEX_POINT('',#5693);
#1871=VERTEX_POINT('',#5697);
#1872=VERTEX_POINT('',#5699);
#1873=VERTEX_POINT('',#5703);
#1874=VERTEX_POINT('',#5705);
#1875=VERTEX_POINT('',#5709);
#1876=VERTEX_POINT('',#5711);
#1877=VERTEX_POINT('',#5715);
#1878=VERTEX_POINT('',#5717);
#1879=VERTEX_POINT('',#5721);
#1880=VERTEX_POINT('',#5723);
#1881=VERTEX_POINT('',#5727);
#1882=VERTEX_POINT('',#5729);
#1883=VERTEX_POINT('',#5733);
#1884=VERTEX_POINT('',#5735);
#1885=VERTEX_POINT('',#5739);
#1886=VERTEX_POINT('',#5741);
#1887=VERTEX_POINT('',#5745);
#1888=VERTEX_POINT('',#5747);
#1889=VERTEX_POINT('',#5754);
#1890=VERTEX_POINT('',#5756);
#1891=VERTEX_POINT('',#5763);
#1892=VERTEX_POINT('',#5765);
#1893=VERTEX_POINT('',#5778);
#1894=VERTEX_POINT('',#5780);
#1895=VERTEX_POINT('',#5784);
#1896=VERTEX_POINT('',#5786);
#1897=VERTEX_POINT('',#5790);
#1898=VERTEX_POINT('',#5792);
#1899=VERTEX_POINT('',#5796);
#1900=VERTEX_POINT('',#5798);
#1901=VERTEX_POINT('',#5802);
#1902=VERTEX_POINT('',#5803);
#1903=VERTEX_POINT('',#5805);
#1904=VERTEX_POINT('',#5807);
#1905=VERTEX_POINT('',#5811);
#1906=VERTEX_POINT('',#5812);
#1907=VERTEX_POINT('',#5817);
#1908=VERTEX_POINT('',#5819);
#1909=VERTEX_POINT('',#5821);
#1910=VERTEX_POINT('',#5823);
#1911=VERTEX_POINT('',#5825);
#1912=VERTEX_POINT('',#5827);
#1913=VERTEX_POINT('',#5831);
#1914=VERTEX_POINT('',#5832);
#1915=VERTEX_POINT('',#5839);
#1916=VERTEX_POINT('',#5841);
#1917=VERTEX_POINT('',#5843);
#1918=VERTEX_POINT('',#5845);
#1919=VERTEX_POINT('',#5853);
#1920=VERTEX_POINT('',#5857);
#1921=VERTEX_POINT('',#5865);
#1922=VERTEX_POINT('',#5866);
#1923=VERTEX_POINT('',#5877);
#1924=VERTEX_POINT('',#5913);
#1925=VERTEX_POINT('',#5943);
#1926=VERTEX_POINT('',#5946);
#1927=VERTEX_POINT('',#5950);
#1928=VERTEX_POINT('',#5954);
#1929=VERTEX_POINT('',#5957);
#1930=VERTEX_POINT('',#5962);
#1931=VERTEX_POINT('',#5968);
#1932=VERTEX_POINT('',#5970);
#1933=VERTEX_POINT('',#5974);
#1934=VERTEX_POINT('',#5976);
#1935=VERTEX_POINT('',#5983);
#1936=VERTEX_POINT('',#5986);
#1937=VERTEX_POINT('',#5987);
#1938=VERTEX_POINT('',#6041);
#1939=VERTEX_POINT('',#6042);
#1940=VERTEX_POINT('',#6046);
#1941=VERTEX_POINT('',#6048);
#1942=VERTEX_POINT('',#6052);
#1943=VERTEX_POINT('',#6059);
#1944=VERTEX_POINT('',#6060);
#1945=VERTEX_POINT('',#6062);
#1946=VERTEX_POINT('',#6064);
#1947=VERTEX_POINT('',#6066);
#1948=VERTEX_POINT('',#6068);
#1949=VERTEX_POINT('',#6072);
#1950=VERTEX_POINT('',#6074);
#1951=VERTEX_POINT('',#6077);
#1952=VERTEX_POINT('',#6079);
#1953=VERTEX_POINT('',#6083);
#1954=VERTEX_POINT('',#6087);
#1955=VERTEX_POINT('',#6091);
#1956=VERTEX_POINT('',#6093);
#1957=VERTEX_POINT('',#6097);
#1958=VERTEX_POINT('',#6099);
#1959=VERTEX_POINT('',#6103);
#1960=VERTEX_POINT('',#6107);
#1961=VERTEX_POINT('',#6115);
#1962=VERTEX_POINT('',#6116);
#1963=VERTEX_POINT('',#6118);
#1964=VERTEX_POINT('',#6120);
#1965=VERTEX_POINT('',#6124);
#1966=VERTEX_POINT('',#6126);
#1967=VERTEX_POINT('',#6130);
#1968=VERTEX_POINT('',#6132);
#1969=VERTEX_POINT('',#6136);
#1970=VERTEX_POINT('',#6138);
#1971=VERTEX_POINT('',#6142);
#1972=VERTEX_POINT('',#6144);
#1973=VERTEX_POINT('',#6153);
#1974=VERTEX_POINT('',#6156);
#1975=VERTEX_POINT('',#6159);
#1976=VERTEX_POINT('',#6163);
#1977=VERTEX_POINT('',#6167);
#1978=VERTEX_POINT('',#6171);
#1979=VERTEX_POINT('',#6174);
#1980=VERTEX_POINT('',#6182);
#1981=VERTEX_POINT('',#6184);
#1982=VERTEX_POINT('',#6188);
#1983=VERTEX_POINT('',#6190);
#1984=VERTEX_POINT('',#6194);
#1985=VERTEX_POINT('',#6196);
#1986=VERTEX_POINT('',#6200);
#1987=VERTEX_POINT('',#6202);
#1988=VERTEX_POINT('',#6206);
#1989=VERTEX_POINT('',#6208);
#1990=VERTEX_POINT('',#6212);
#1991=VERTEX_POINT('',#6213);
#1992=VERTEX_POINT('',#6215);
#1993=VERTEX_POINT('',#6217);
#1994=VERTEX_POINT('',#6221);
#1995=VERTEX_POINT('',#6223);
#1996=VERTEX_POINT('',#6227);
#1997=VERTEX_POINT('',#6229);
#1998=VERTEX_POINT('',#6239);
#1999=VERTEX_POINT('',#6241);
#2000=VERTEX_POINT('',#6245);
#2001=VERTEX_POINT('',#6247);
#2002=VERTEX_POINT('',#6251);
#2003=VERTEX_POINT('',#6253);
#2004=VERTEX_POINT('',#6257);
#2005=VERTEX_POINT('',#6258);
#2006=VERTEX_POINT('',#6260);
#2007=VERTEX_POINT('',#6262);
#2008=VERTEX_POINT('',#6266);
#2009=VERTEX_POINT('',#6267);
#2010=VERTEX_POINT('',#6269);
#2011=VERTEX_POINT('',#6271);
#2012=VERTEX_POINT('',#6275);
#2013=VERTEX_POINT('',#6277);
#2014=VERTEX_POINT('',#6281);
#2015=VERTEX_POINT('',#6283);
#2016=VERTEX_POINT('',#6290);
#2017=VERTEX_POINT('',#6292);
#2018=VERTEX_POINT('',#6296);
#2019=VERTEX_POINT('',#6300);
#2020=VERTEX_POINT('',#6308);
#2021=VERTEX_POINT('',#6311);
#2022=VERTEX_POINT('',#6315);
#2023=VERTEX_POINT('',#6319);
#2024=VERTEX_POINT('',#6323);
#2025=VERTEX_POINT('',#6326);
#2026=VERTEX_POINT('',#6330);
#2027=VERTEX_POINT('',#6334);
#2028=VERTEX_POINT('',#6339);
#2029=VERTEX_POINT('',#6340);
#2030=VERTEX_POINT('',#6342);
#2031=VERTEX_POINT('',#6344);
#2032=VERTEX_POINT('',#6348);
#2033=VERTEX_POINT('',#6350);
#2034=VERTEX_POINT('',#6354);
#2035=VERTEX_POINT('',#6356);
#2036=VERTEX_POINT('',#6360);
#2037=VERTEX_POINT('',#6362);
#2038=VERTEX_POINT('',#6366);
#2039=VERTEX_POINT('',#6368);
#2040=VERTEX_POINT('',#6378);
#2041=VERTEX_POINT('',#6379);
#2042=VERTEX_POINT('',#6383);
#2043=VERTEX_POINT('',#6387);
#2044=VERTEX_POINT('',#6390);
#2045=VERTEX_POINT('',#6394);
#2046=VERTEX_POINT('',#6398);
#2047=VERTEX_POINT('',#6406);
#2048=VERTEX_POINT('',#6408);
#2049=VERTEX_POINT('',#6410);
#2050=VERTEX_POINT('',#6414);
#2051=VERTEX_POINT('',#6418);
#2052=VERTEX_POINT('',#6422);
#2053=VERTEX_POINT('',#6426);
#2054=VERTEX_POINT('',#6441);
#2055=VERTEX_POINT('',#6443);
#2056=VERTEX_POINT('',#6455);
#2057=VERTEX_POINT('',#6457);
#2058=VERTEX_POINT('',#6461);
#2059=VERTEX_POINT('',#6465);
#2060=VERTEX_POINT('',#6468);
#2061=VERTEX_POINT('',#6505);
#2062=VERTEX_POINT('',#6508);
#2063=VERTEX_POINT('',#6512);
#2064=VERTEX_POINT('',#6516);
#2065=VERTEX_POINT('',#6520);
#2066=VERTEX_POINT('',#6523);
#2067=VERTEX_POINT('',#6527);
#2068=VERTEX_POINT('',#6531);
#2069=VERTEX_POINT('',#6536);
#2070=VERTEX_POINT('',#6537);
#2071=VERTEX_POINT('',#6539);
#2072=VERTEX_POINT('',#6541);
#2073=VERTEX_POINT('',#6545);
#2074=VERTEX_POINT('',#6547);
#2075=VERTEX_POINT('',#6551);
#2076=VERTEX_POINT('',#6553);
#2077=VERTEX_POINT('',#6557);
#2078=VERTEX_POINT('',#6559);
#2079=VERTEX_POINT('',#6563);
#2080=VERTEX_POINT('',#6565);
#2081=VERTEX_POINT('',#6575);
#2082=VERTEX_POINT('',#6576);
#2083=VERTEX_POINT('',#6580);
#2084=VERTEX_POINT('',#6584);
#2085=VERTEX_POINT('',#6587);
#2086=VERTEX_POINT('',#6591);
#2087=VERTEX_POINT('',#6595);
#2088=VERTEX_POINT('',#6603);
#2089=VERTEX_POINT('',#6605);
#2090=VERTEX_POINT('',#6607);
#2091=VERTEX_POINT('',#6611);
#2092=VERTEX_POINT('',#6615);
#2093=VERTEX_POINT('',#6619);
#2094=VERTEX_POINT('',#6623);
#2095=VERTEX_POINT('',#6638);
#2096=VERTEX_POINT('',#6640);
#2097=VERTEX_POINT('',#6667);
#2098=VERTEX_POINT('',#6669);
#2099=VERTEX_POINT('',#6673);
#2100=VERTEX_POINT('',#6674);
#2101=VERTEX_POINT('',#6676);
#2102=VERTEX_POINT('',#6678);
#2103=VERTEX_POINT('',#6682);
#2104=VERTEX_POINT('',#6684);
#2105=VERTEX_POINT('',#6688);
#2106=VERTEX_POINT('',#6690);
#2107=EDGE_CURVE('',#1791,#1791,#1698,.T.);
#2108=EDGE_CURVE('',#1791,#1792,#982,.T.);
#2109=EDGE_CURVE('',#1792,#1792,#1699,.T.);
#2110=EDGE_CURVE('',#1793,#1793,#1700,.T.);
#2111=EDGE_CURVE('',#1793,#1794,#983,.T.);
#2112=EDGE_CURVE('',#1794,#1794,#1701,.T.);
#2113=EDGE_CURVE('',#1795,#1796,#984,.T.);
#2114=EDGE_CURVE('',#1796,#1797,#985,.T.);
#2115=EDGE_CURVE('',#1798,#1797,#986,.T.);
#2116=EDGE_CURVE('',#1795,#1798,#987,.T.);
#2117=EDGE_CURVE('',#1799,#1795,#988,.T.);
#2118=EDGE_CURVE('',#1800,#1798,#989,.T.);
#2119=EDGE_CURVE('',#1799,#1800,#990,.T.);
#2120=EDGE_CURVE('',#1801,#1799,#991,.T.);
#2121=EDGE_CURVE('',#1802,#1800,#992,.T.);
#2122=EDGE_CURVE('',#1801,#1802,#993,.T.);
#2123=EDGE_CURVE('',#1796,#1801,#994,.T.);
#2124=EDGE_CURVE('',#1797,#1802,#995,.T.);
#2125=EDGE_CURVE('',#1803,#1804,#996,.T.);
#2126=EDGE_CURVE('',#1803,#1805,#997,.T.);
#2127=EDGE_CURVE('',#1806,#1805,#998,.T.);
#2128=EDGE_CURVE('',#1804,#1806,#999,.T.);
#2129=EDGE_CURVE('',#1807,#1803,#1000,.T.);
#2130=EDGE_CURVE('',#1807,#1808,#1001,.T.);
#2131=EDGE_CURVE('',#1805,#1808,#1002,.T.);
#2132=EDGE_CURVE('',#1809,#1807,#1003,.T.);
#2133=EDGE_CURVE('',#1809,#1810,#1004,.T.);
#2134=EDGE_CURVE('',#1808,#1810,#1005,.T.);
#2135=EDGE_CURVE('',#1811,#1809,#1006,.T.);
#2136=EDGE_CURVE('',#1811,#1812,#1007,.T.);
#2137=EDGE_CURVE('',#1810,#1812,#1008,.T.);
#2138=EDGE_CURVE('',#1813,#1811,#1009,.T.);
#2139=EDGE_CURVE('',#1813,#1814,#1010,.T.);
#2140=EDGE_CURVE('',#1812,#1814,#1011,.T.);
#2141=EDGE_CURVE('',#1815,#1813,#1012,.T.);
#2142=EDGE_CURVE('',#1815,#1816,#1013,.T.);
#2143=EDGE_CURVE('',#1814,#1816,#1014,.T.);
#2144=EDGE_CURVE('',#1817,#1815,#1015,.T.);
#2145=EDGE_CURVE('',#1817,#1818,#1016,.T.);
#2146=EDGE_CURVE('',#1816,#1818,#1017,.T.);
#2147=EDGE_CURVE('',#1819,#1817,#1018,.T.);
#2148=EDGE_CURVE('',#1819,#1820,#1019,.T.);
#2149=EDGE_CURVE('',#1818,#1820,#1020,.T.);
#2150=EDGE_CURVE('',#1821,#1819,#1021,.T.);
#2151=EDGE_CURVE('',#1822,#1821,#1022,.T.);
#2152=EDGE_CURVE('',#1820,#1822,#1023,.T.);
#2153=EDGE_CURVE('',#1823,#1824,#1024,.T.);
#2154=EDGE_CURVE('',#1823,#1825,#1025,.T.);
#2155=EDGE_CURVE('',#1826,#1825,#1026,.T.);
#2156=EDGE_CURVE('',#1824,#1826,#1027,.T.);
#2157=EDGE_CURVE('',#1827,#1823,#1028,.T.);
#2158=EDGE_CURVE('',#1827,#1828,#1029,.T.);
#2159=EDGE_CURVE('',#1825,#1828,#1030,.T.);
#2160=EDGE_CURVE('',#1829,#1827,#1031,.T.);
#2161=EDGE_CURVE('',#1829,#1830,#1032,.T.);
#2162=EDGE_CURVE('',#1828,#1830,#1033,.T.);
#2163=EDGE_CURVE('',#1831,#1829,#1034,.T.);
#2164=EDGE_CURVE('',#1831,#1832,#1035,.T.);
#2165=EDGE_CURVE('',#1830,#1832,#1036,.T.);
#2166=EDGE_CURVE('',#1833,#1831,#1037,.T.);
#2167=EDGE_CURVE('',#1833,#1834,#1038,.T.);
#2168=EDGE_CURVE('',#1832,#1834,#1039,.T.);
#2169=EDGE_CURVE('',#1835,#1833,#1040,.T.);
#2170=EDGE_CURVE('',#1835,#1836,#1041,.T.);
#2171=EDGE_CURVE('',#1834,#1836,#1042,.T.);
#2172=EDGE_CURVE('',#1837,#1835,#1043,.T.);
#2173=EDGE_CURVE('',#1837,#1838,#1044,.T.);
#2174=EDGE_CURVE('',#1836,#1838,#1045,.T.);
#2175=EDGE_CURVE('',#1839,#1837,#1046,.T.);
#2176=EDGE_CURVE('',#1839,#1840,#1047,.T.);
#2177=EDGE_CURVE('',#1838,#1840,#1048,.T.);
#2178=EDGE_CURVE('',#1841,#1839,#1049,.T.);
#2179=EDGE_CURVE('',#1842,#1841,#1050,.T.);
#2180=EDGE_CURVE('',#1840,#1842,#1051,.T.);
#2181=EDGE_CURVE('',#1843,#1844,#1052,.T.);
#2182=EDGE_CURVE('',#1843,#1845,#1053,.T.);
#2183=EDGE_CURVE('',#1846,#1845,#1054,.T.);
#2184=EDGE_CURVE('',#1844,#1846,#1055,.T.);
#2185=EDGE_CURVE('',#1847,#1843,#1056,.T.);
#2186=EDGE_CURVE('',#1847,#1848,#1057,.T.);
#2187=EDGE_CURVE('',#1845,#1848,#1058,.T.);
#2188=EDGE_CURVE('',#1849,#1847,#1059,.T.);
#2189=EDGE_CURVE('',#1849,#1850,#1060,.T.);
#2190=EDGE_CURVE('',#1848,#1850,#1061,.T.);
#2191=EDGE_CURVE('',#1851,#1849,#1062,.T.);
#2192=EDGE_CURVE('',#1851,#1852,#1063,.T.);
#2193=EDGE_CURVE('',#1850,#1852,#1064,.T.);
#2194=EDGE_CURVE('',#1853,#1851,#1065,.T.);
#2195=EDGE_CURVE('',#1853,#1854,#1066,.T.);
#2196=EDGE_CURVE('',#1852,#1854,#1067,.T.);
#2197=EDGE_CURVE('',#1855,#1853,#1068,.T.);
#2198=EDGE_CURVE('',#1855,#1856,#1069,.T.);
#2199=EDGE_CURVE('',#1854,#1856,#1070,.T.);
#2200=EDGE_CURVE('',#1857,#1855,#1071,.T.);
#2201=EDGE_CURVE('',#1857,#1858,#1072,.T.);
#2202=EDGE_CURVE('',#1856,#1858,#1073,.T.);
#2203=EDGE_CURVE('',#1859,#1857,#1074,.T.);
#2204=EDGE_CURVE('',#1859,#1860,#1075,.T.);
#2205=EDGE_CURVE('',#1858,#1860,#1076,.T.);
#2206=EDGE_CURVE('',#1861,#1859,#1077,.T.);
#2207=EDGE_CURVE('',#1862,#1861,#1078,.T.);
#2208=EDGE_CURVE('',#1860,#1862,#1079,.T.);
#2209=EDGE_CURVE('',#1863,#1864,#1080,.T.);
#2210=EDGE_CURVE('',#1863,#1865,#1081,.T.);
#2211=EDGE_CURVE('',#1866,#1865,#1082,.T.);
#2212=EDGE_CURVE('',#1864,#1866,#1083,.T.);
#2213=EDGE_CURVE('',#1867,#1863,#1084,.T.);
#2214=EDGE_CURVE('',#1867,#1868,#1085,.T.);
#2215=EDGE_CURVE('',#1865,#1868,#1086,.T.);
#2216=EDGE_CURVE('',#1869,#1867,#1087,.T.);
#2217=EDGE_CURVE('',#1869,#1870,#1088,.T.);
#2218=EDGE_CURVE('',#1868,#1870,#1089,.T.);
#2219=EDGE_CURVE('',#1871,#1869,#1090,.T.);
#2220=EDGE_CURVE('',#1871,#1872,#1091,.T.);
#2221=EDGE_CURVE('',#1870,#1872,#1092,.T.);
#2222=EDGE_CURVE('',#1873,#1871,#1093,.T.);
#2223=EDGE_CURVE('',#1873,#1874,#1094,.T.);
#2224=EDGE_CURVE('',#1872,#1874,#1095,.T.);
#2225=EDGE_CURVE('',#1875,#1873,#1096,.T.);
#2226=EDGE_CURVE('',#1875,#1876,#1097,.T.);
#2227=EDGE_CURVE('',#1874,#1876,#1098,.T.);
#2228=EDGE_CURVE('',#1877,#1875,#1099,.T.);
#2229=EDGE_CURVE('',#1877,#1878,#1100,.T.);
#2230=EDGE_CURVE('',#1876,#1878,#1101,.T.);
#2231=EDGE_CURVE('',#1879,#1877,#1102,.T.);
#2232=EDGE_CURVE('',#1879,#1880,#1103,.T.);
#2233=EDGE_CURVE('',#1878,#1880,#1104,.T.);
#2234=EDGE_CURVE('',#1881,#1879,#1105,.T.);
#2235=EDGE_CURVE('',#1882,#1881,#1106,.T.);
#2236=EDGE_CURVE('',#1880,#1882,#1107,.T.);
#2237=EDGE_CURVE('',#1883,#1883,#1702,.T.);
#2238=EDGE_CURVE('',#1883,#1884,#1108,.T.);
#2239=EDGE_CURVE('',#1884,#1884,#1703,.T.);
#2240=EDGE_CURVE('',#1821,#1885,#1109,.T.);
#2241=EDGE_CURVE('',#1885,#1886,#1110,.T.);
#2242=EDGE_CURVE('',#1822,#1886,#1111,.T.);
#2243=EDGE_CURVE('',#1887,#1806,#1112,.T.);
#2244=EDGE_CURVE('',#1888,#1887,#1113,.T.);
#2245=EDGE_CURVE('',#1888,#1804,#1114,.T.);
#2246=EDGE_CURVE('',#1841,#1888,#1115,.T.);
#2247=EDGE_CURVE('',#1842,#1887,#1116,.T.);
#2248=EDGE_CURVE('',#1889,#1826,#1117,.T.);
#2249=EDGE_CURVE('',#1890,#1889,#1118,.T.);
#2250=EDGE_CURVE('',#1890,#1824,#1119,.T.);
#2251=EDGE_CURVE('',#1861,#1890,#1120,.T.);
#2252=EDGE_CURVE('',#1862,#1889,#1121,.T.);
#2253=EDGE_CURVE('',#1891,#1846,#1122,.T.);
#2254=EDGE_CURVE('',#1892,#1891,#1123,.T.);
#2255=EDGE_CURVE('',#1892,#1844,#1124,.T.);
#2256=EDGE_CURVE('',#1881,#1892,#1125,.T.);
#2257=EDGE_CURVE('',#1882,#1891,#1126,.T.);
#2258=EDGE_CURVE('',#1886,#1866,#1127,.T.);
#2259=EDGE_CURVE('',#1885,#1864,#1128,.T.);
#2260=EDGE_CURVE('',#1893,#1893,#1704,.T.);
#2261=EDGE_CURVE('',#1893,#1894,#1129,.T.);
#2262=EDGE_CURVE('',#1894,#1894,#1705,.T.);
#2263=EDGE_CURVE('',#1895,#1895,#1706,.T.);
#2264=EDGE_CURVE('',#1895,#1896,#1130,.T.);
#2265=EDGE_CURVE('',#1896,#1896,#1707,.T.);
#2266=EDGE_CURVE('',#1897,#1897,#1708,.T.);
#2267=EDGE_CURVE('',#1897,#1898,#1131,.T.);
#2268=EDGE_CURVE('',#1898,#1898,#1709,.T.);
#2269=EDGE_CURVE('',#1899,#1899,#1710,.T.);
#2270=EDGE_CURVE('',#1899,#1900,#1132,.T.);
#2271=EDGE_CURVE('',#1900,#1900,#1711,.T.);
#2272=EDGE_CURVE('',#1901,#1902,#1133,.T.);
#2273=EDGE_CURVE('',#1903,#1901,#1134,.T.);
#2274=EDGE_CURVE('',#1903,#1904,#1135,.T.);
#2275=EDGE_CURVE('',#1904,#1902,#1136,.T.);
#2276=EDGE_CURVE('',#1905,#1906,#1137,.T.);
#2277=EDGE_CURVE('',#1905,#1904,#1138,.T.);
#2278=EDGE_CURVE('',#1906,#1903,#1139,.T.);
#2279=EDGE_CURVE('',#1907,#1901,#1140,.T.);
#2280=EDGE_CURVE('',#1902,#1908,#1141,.T.);
#2281=EDGE_CURVE('',#1908,#1909,#1142,.T.);
#2282=EDGE_CURVE('',#1910,#1909,#1143,.T.);
#2283=EDGE_CURVE('',#1911,#1910,#1144,.T.);
#2284=EDGE_CURVE('',#1911,#1912,#1145,.T.);
#2285=EDGE_CURVE('',#1912,#1907,#1146,.T.);
#2286=EDGE_CURVE('',#1913,#1914,#1147,.T.);
#2287=EDGE_CURVE('',#1909,#1913,#1712,.T.);
#2288=EDGE_CURVE('',#1908,#1914,#1713,.T.);
#2289=EDGE_CURVE('',#1914,#1905,#1148,.T.);
#2290=EDGE_CURVE('',#1906,#1915,#1149,.T.);
#2291=EDGE_CURVE('',#1915,#1916,#1150,.T.);
#2292=EDGE_CURVE('',#1916,#1917,#1151,.T.);
#2293=EDGE_CURVE('',#1917,#1918,#1152,.T.);
#2294=EDGE_CURVE('',#1913,#1918,#1153,.T.);
#2295=EDGE_CURVE('',#1907,#1915,#1714,.T.);
#2296=EDGE_CURVE('',#1912,#1916,#1715,.T.);
#2297=EDGE_CURVE('',#1919,#1911,#1154,.T.);
#2298=EDGE_CURVE('',#1917,#1919,#1155,.T.);
#2299=EDGE_CURVE('',#1919,#1920,#1156,.T.);
#2300=EDGE_CURVE('',#1918,#1920,#1157,.T.);
#2301=EDGE_CURVE('',#1920,#1910,#1158,.T.);
#2302=EDGE_CURVE('',#1921,#1922,#258,.T.);
#2303=EDGE_CURVE('',#1921,#1923,#1159,.T.);
#2304=EDGE_CURVE('',#1923,#1923,#259,.T.);
#2305=EDGE_CURVE('',#1924,#1921,#260,.T.);
#2306=EDGE_CURVE('',#1922,#1924,#261,.T.);
#2307=EDGE_CURVE('',#1925,#1925,#1716,.T.);
#2308=EDGE_CURVE('',#1926,#1926,#1717,.T.);
#2309=EDGE_CURVE('',#1926,#1925,#1160,.T.);
#2310=EDGE_CURVE('',#1927,#1927,#1718,.T.);
#2311=EDGE_CURVE('',#1927,#1926,#1161,.T.);
#2312=EDGE_CURVE('',#1928,#1928,#1719,.T.);
#2313=EDGE_CURVE('',#1929,#1929,#1720,.T.);
#2314=EDGE_CURVE('',#1929,#1922,#1162,.T.);
#2315=EDGE_CURVE('',#1924,#1928,#1163,.T.);
#2316=EDGE_CURVE('',#1930,#1930,#1721,.T.);
#2317=EDGE_CURVE('',#1930,#1929,#1164,.T.);
#2318=EDGE_CURVE('',#1931,#1931,#1722,.T.);
#2319=EDGE_CURVE('',#1931,#1932,#1165,.T.);
#2320=EDGE_CURVE('',#1932,#1932,#1723,.T.);
#2321=EDGE_CURVE('',#1933,#1933,#1724,.T.);
#2322=EDGE_CURVE('',#1933,#1934,#1166,.T.);
#2323=EDGE_CURVE('',#1934,#1934,#1725,.T.);
#2324=EDGE_CURVE('',#1935,#1935,#1726,.T.);
#2325=EDGE_CURVE('',#1935,#1935,#1727,.T.);
#2326=EDGE_CURVE('',#1936,#1937,#262,.T.);
#2327=EDGE_CURVE('',#1937,#1936,#263,.T.);
#2328=EDGE_CURVE('',#1938,#1939,#1728,.T.);
#2329=EDGE_CURVE('',#1938,#1939,#1167,.T.);
#2330=EDGE_CURVE('',#1939,#1940,#1168,.T.);
#2331=EDGE_CURVE('',#1941,#1940,#1169,.T.);
#2332=EDGE_CURVE('',#1938,#1941,#1170,.T.);
#2333=EDGE_CURVE('',#1942,#1941,#1729,.T.);
#2334=EDGE_CURVE('',#1942,#1937,#1171,.T.);
#2335=EDGE_CURVE('',#1940,#1942,#1730,.T.);
#2336=EDGE_CURVE('',#1943,#1944,#1172,.T.);
#2337=EDGE_CURVE('',#1944,#1945,#1173,.T.);
#2338=EDGE_CURVE('',#1945,#1946,#1174,.T.);
#2339=EDGE_CURVE('',#1946,#1947,#1175,.T.);
#2340=EDGE_CURVE('',#1947,#1948,#237,.T.);
#2341=EDGE_CURVE('',#1948,#1943,#1176,.T.);
#2342=EDGE_CURVE('',#1949,#1947,#1731,.F.);
#2343=EDGE_CURVE('',#1949,#1950,#1177,.T.);
#2344=EDGE_CURVE('',#1950,#1950,#1732,.T.);
#2345=EDGE_CURVE('',#1951,#1949,#1733,.F.);
#2346=EDGE_CURVE('',#1952,#1951,#238,.T.);
#2347=EDGE_CURVE('',#1948,#1952,#1734,.F.);
#2348=EDGE_CURVE('',#1953,#1946,#1178,.T.);
#2349=EDGE_CURVE('',#1951,#1953,#1179,.T.);
#2350=EDGE_CURVE('',#1954,#1952,#1180,.T.);
#2351=EDGE_CURVE('',#1943,#1954,#1181,.T.);
#2352=EDGE_CURVE('',#1953,#1955,#1182,.T.);
#2353=EDGE_CURVE('',#1955,#1956,#1183,.T.);
#2354=EDGE_CURVE('',#1956,#1954,#1184,.T.);
#2355=EDGE_CURVE('',#1956,#1957,#1185,.T.);
#2356=EDGE_CURVE('',#1958,#1957,#1186,.T.);
#2357=EDGE_CURVE('',#1944,#1958,#1187,.T.);
#2358=EDGE_CURVE('',#1955,#1959,#1188,.T.);
#2359=EDGE_CURVE('',#1957,#1959,#1189,.T.);
#2360=EDGE_CURVE('',#1960,#1958,#1190,.T.);
#2361=EDGE_CURVE('',#1945,#1960,#1191,.T.);
#2362=EDGE_CURVE('',#1959,#1960,#1192,.T.);
#2363=EDGE_CURVE('',#1961,#1962,#1193,.T.);
#2364=EDGE_CURVE('',#1962,#1963,#1194,.T.);
#2365=EDGE_CURVE('',#1963,#1964,#1195,.T.);
#2366=EDGE_CURVE('',#1961,#1964,#1196,.T.);
#2367=EDGE_CURVE('',#1962,#1965,#1197,.T.);
#2368=EDGE_CURVE('',#1965,#1966,#1198,.T.);
#2369=EDGE_CURVE('',#1966,#1963,#1199,.T.);
#2370=EDGE_CURVE('',#1965,#1967,#1200,.T.);
#2371=EDGE_CURVE('',#1967,#1968,#1201,.T.);
#2372=EDGE_CURVE('',#1968,#1966,#1202,.T.);
#2373=EDGE_CURVE('',#1967,#1969,#1203,.T.);
#2374=EDGE_CURVE('',#1969,#1970,#1204,.T.);
#2375=EDGE_CURVE('',#1970,#1968,#1205,.T.);
#2376=EDGE_CURVE('',#1969,#1971,#1206,.T.);
#2377=EDGE_CURVE('',#1971,#1972,#1207,.T.);
#2378=EDGE_CURVE('',#1972,#1970,#1208,.T.);
#2379=EDGE_CURVE('',#1971,#1961,#1209,.T.);
#2380=EDGE_CURVE('',#1964,#1972,#1210,.T.);
#2381=EDGE_CURVE('',#1973,#1973,#1735,.T.);
#2382=EDGE_CURVE('',#1974,#1974,#1736,.T.);
#2383=EDGE_CURVE('',#1975,#1975,#1737,.T.);
#2384=EDGE_CURVE('',#1975,#1974,#1211,.T.);
#2385=EDGE_CURVE('',#1976,#1976,#1738,.T.);
#2386=EDGE_CURVE('',#1976,#1975,#1212,.T.);
#2387=EDGE_CURVE('',#1977,#1977,#1739,.T.);
#2388=EDGE_CURVE('',#1977,#1976,#1213,.T.);
#2389=EDGE_CURVE('',#1978,#1978,#1740,.T.);
#2390=EDGE_CURVE('',#1979,#1979,#1741,.F.);
#2391=EDGE_CURVE('',#1979,#1978,#1214,.T.);
#2392=EDGE_CURVE('',#1973,#1979,#1215,.T.);
#2393=EDGE_CURVE('',#1980,#1980,#1742,.T.);
#2394=EDGE_CURVE('',#1980,#1981,#1216,.T.);
#2395=EDGE_CURVE('',#1981,#1981,#1743,.T.);
#2396=EDGE_CURVE('',#1982,#1982,#1744,.T.);
#2397=EDGE_CURVE('',#1982,#1983,#1217,.T.);
#2398=EDGE_CURVE('',#1983,#1983,#1745,.T.);
#2399=EDGE_CURVE('',#1984,#1984,#1746,.T.);
#2400=EDGE_CURVE('',#1984,#1985,#1218,.T.);
#2401=EDGE_CURVE('',#1985,#1985,#1747,.T.);
#2402=EDGE_CURVE('',#1986,#1986,#1748,.T.);
#2403=EDGE_CURVE('',#1986,#1987,#1219,.T.);
#2404=EDGE_CURVE('',#1987,#1987,#1749,.T.);
#2405=EDGE_CURVE('',#1988,#1988,#1750,.T.);
#2406=EDGE_CURVE('',#1988,#1989,#1220,.T.);
#2407=EDGE_CURVE('',#1989,#1989,#1751,.T.);
#2408=EDGE_CURVE('',#1990,#1991,#1221,.T.);
#2409=EDGE_CURVE('',#1991,#1992,#1222,.T.);
#2410=EDGE_CURVE('',#1993,#1992,#1223,.T.);
#2411=EDGE_CURVE('',#1990,#1993,#1224,.T.);
#2412=EDGE_CURVE('',#1994,#1990,#1225,.T.);
#2413=EDGE_CURVE('',#1995,#1993,#1226,.T.);
#2414=EDGE_CURVE('',#1994,#1995,#1227,.T.);
#2415=EDGE_CURVE('',#1996,#1994,#1228,.T.);
#2416=EDGE_CURVE('',#1997,#1995,#1229,.T.);
#2417=EDGE_CURVE('',#1996,#1997,#1230,.T.);
#2418=EDGE_CURVE('',#1991,#1996,#1231,.T.);
#2419=EDGE_CURVE('',#1992,#1997,#1232,.T.);
#2420=EDGE_CURVE('',#1998,#1998,#1752,.T.);
#2421=EDGE_CURVE('',#1998,#1999,#1233,.T.);
#2422=EDGE_CURVE('',#1999,#1999,#1753,.T.);
#2423=EDGE_CURVE('',#2000,#2000,#1754,.T.);
#2424=EDGE_CURVE('',#2000,#2001,#1234,.T.);
#2425=EDGE_CURVE('',#2001,#2001,#1755,.T.);
#2426=EDGE_CURVE('',#2002,#2002,#1756,.T.);
#2427=EDGE_CURVE('',#2002,#2003,#1235,.T.);
#2428=EDGE_CURVE('',#2003,#2003,#1757,.T.);
#2429=EDGE_CURVE('',#2004,#2005,#1236,.T.);
#2430=EDGE_CURVE('',#2006,#2004,#1237,.T.);
#2431=EDGE_CURVE('',#2006,#2007,#1238,.T.);
#2432=EDGE_CURVE('',#2005,#2007,#1239,.T.);
#2433=EDGE_CURVE('',#2008,#2009,#1240,.T.);
#2434=EDGE_CURVE('',#2010,#2008,#1241,.T.);
#2435=EDGE_CURVE('',#2011,#2010,#1242,.T.);
#2436=EDGE_CURVE('',#2009,#2011,#1243,.T.);
#2437=EDGE_CURVE('',#2011,#2012,#1244,.T.);
#2438=EDGE_CURVE('',#2013,#2010,#1245,.T.);
#2439=EDGE_CURVE('',#2012,#2013,#1246,.T.);
#2440=EDGE_CURVE('',#2012,#2014,#1247,.T.);
#2441=EDGE_CURVE('',#2015,#2013,#1248,.T.);
#2442=EDGE_CURVE('',#2014,#2015,#1249,.T.);
#2443=EDGE_CURVE('',#2014,#2006,#1250,.T.);
#2444=EDGE_CURVE('',#2007,#2015,#1251,.T.);
#2445=EDGE_CURVE('',#2016,#2009,#1252,.T.);
#2446=EDGE_CURVE('',#2017,#2016,#1758,.T.);
#2447=EDGE_CURVE('',#2008,#2017,#1253,.T.);
#2448=EDGE_CURVE('',#2004,#2018,#1254,.T.);
#2449=EDGE_CURVE('',#2016,#2018,#1255,.T.);
#2450=EDGE_CURVE('',#2019,#2017,#1256,.T.);
#2451=EDGE_CURVE('',#2019,#2005,#1257,.T.);
#2452=EDGE_CURVE('',#2019,#2018,#1759,.T.);
#2453=EDGE_CURVE('',#2020,#2020,#1760,.T.);
#2454=EDGE_CURVE('',#2021,#2021,#1761,.T.);
#2455=EDGE_CURVE('',#2021,#2020,#1258,.T.);
#2456=EDGE_CURVE('',#2022,#2022,#1762,.T.);
#2457=EDGE_CURVE('',#2022,#2021,#1259,.T.);
#2458=EDGE_CURVE('',#2023,#2023,#1763,.T.);
#2459=EDGE_CURVE('',#2023,#2022,#1260,.T.);
#2460=EDGE_CURVE('',#2024,#2024,#1764,.T.);
#2461=EDGE_CURVE('',#2025,#2025,#1765,.F.);
#2462=EDGE_CURVE('',#2025,#2024,#1261,.T.);
#2463=EDGE_CURVE('',#2026,#2026,#1766,.F.);
#2464=EDGE_CURVE('',#2026,#2025,#1262,.T.);
#2465=EDGE_CURVE('',#2027,#2027,#1767,.T.);
#2466=EDGE_CURVE('',#2027,#2026,#1263,.T.);
#2467=EDGE_CURVE('',#2028,#2029,#1264,.T.);
#2468=EDGE_CURVE('',#2029,#2030,#1265,.T.);
#2469=EDGE_CURVE('',#2030,#2031,#1266,.T.);
#2470=EDGE_CURVE('',#2028,#2031,#1267,.T.);
#2471=EDGE_CURVE('',#2029,#2032,#1268,.T.);
#2472=EDGE_CURVE('',#2032,#2033,#1269,.T.);
#2473=EDGE_CURVE('',#2033,#2030,#1270,.T.);
#2474=EDGE_CURVE('',#2032,#2034,#1271,.T.);
#2475=EDGE_CURVE('',#2034,#2035,#1272,.T.);
#2476=EDGE_CURVE('',#2035,#2033,#1273,.T.);
#2477=EDGE_CURVE('',#2034,#2036,#1274,.T.);
#2478=EDGE_CURVE('',#2036,#2037,#1275,.T.);
#2479=EDGE_CURVE('',#2037,#2035,#1276,.T.);
#2480=EDGE_CURVE('',#2036,#2038,#1277,.T.);
#2481=EDGE_CURVE('',#2038,#2039,#1278,.T.);
#2482=EDGE_CURVE('',#2039,#2037,#1279,.T.);
#2483=EDGE_CURVE('',#2038,#2028,#1280,.T.);
#2484=EDGE_CURVE('',#2031,#2039,#1281,.T.);
#2485=EDGE_CURVE('',#2040,#2041,#207,.T.);
#2486=EDGE_CURVE('',#2042,#2040,#208,.T.);
#2487=EDGE_CURVE('',#2042,#2043,#1282,.T.);
#2488=EDGE_CURVE('',#2043,#2043,#1768,.T.);
#2489=EDGE_CURVE('',#2044,#2042,#209,.T.);
#2490=EDGE_CURVE('',#2045,#2044,#210,.T.);
#2491=EDGE_CURVE('',#2046,#2045,#211,.T.);
#2492=EDGE_CURVE('',#2041,#2046,#212,.T.);
#2493=EDGE_CURVE('',#2047,#2047,#1769,.T.);
#2494=EDGE_CURVE('',#2047,#2048,#1283,.T.);
#2495=EDGE_CURVE('',#2049,#2048,#213,.T.);
#2496=EDGE_CURVE('',#2050,#2049,#214,.T.);
#2497=EDGE_CURVE('',#2051,#2050,#215,.T.);
#2498=EDGE_CURVE('',#2052,#2051,#216,.T.);
#2499=EDGE_CURVE('',#2053,#2052,#217,.T.);
#2500=EDGE_CURVE('',#2048,#2053,#218,.T.);
#2501=EDGE_CURVE('',#2044,#2053,#1284,.T.);
#2502=EDGE_CURVE('',#2045,#2052,#1285,.T.);
#2503=EDGE_CURVE('',#2042,#2048,#1286,.T.);
#2504=EDGE_CURVE('',#2040,#2049,#1287,.T.);
#2505=EDGE_CURVE('',#2054,#2054,#1770,.F.);
#2506=EDGE_CURVE('',#2054,#2055,#1288,.T.);
#2507=EDGE_CURVE('',#2055,#2055,#1771,.F.);
#2508=EDGE_CURVE('',#2041,#2050,#1289,.T.);
#2509=EDGE_CURVE('',#2046,#2051,#1290,.T.);
#2510=EDGE_CURVE('',#2056,#2056,#1772,.T.);
#2511=EDGE_CURVE('',#2056,#2057,#1291,.T.);
#2512=EDGE_CURVE('',#2057,#2057,#1773,.T.);
#2513=EDGE_CURVE('',#2057,#2058,#1292,.T.);
#2514=EDGE_CURVE('',#2058,#2058,#1774,.T.);
#2515=EDGE_CURVE('',#2059,#2059,#1775,.T.);
#2516=EDGE_CURVE('',#2059,#2060,#1293,.T.);
#2517=EDGE_CURVE('',#2060,#2060,#1776,.T.);
#2518=EDGE_CURVE('',#2061,#2061,#1777,.T.);
#2519=EDGE_CURVE('',#2062,#2062,#1778,.T.);
#2520=EDGE_CURVE('',#2062,#2061,#1294,.T.);
#2521=EDGE_CURVE('',#2063,#2063,#1779,.T.);
#2522=EDGE_CURVE('',#2063,#2062,#1295,.T.);
#2523=EDGE_CURVE('',#2064,#2064,#1780,.T.);
#2524=EDGE_CURVE('',#2064,#2063,#1296,.T.);
#2525=EDGE_CURVE('',#2065,#2065,#1781,.T.);
#2526=EDGE_CURVE('',#2066,#2066,#1782,.F.);
#2527=EDGE_CURVE('',#2066,#2065,#1297,.T.);
#2528=EDGE_CURVE('',#2067,#2067,#1783,.F.);
#2529=EDGE_CURVE('',#2067,#2066,#1298,.T.);
#2530=EDGE_CURVE('',#2068,#2068,#1784,.T.);
#2531=EDGE_CURVE('',#2068,#2067,#1299,.T.);
#2532=EDGE_CURVE('',#2069,#2070,#1300,.T.);
#2533=EDGE_CURVE('',#2070,#2071,#1301,.T.);
#2534=EDGE_CURVE('',#2071,#2072,#1302,.T.);
#2535=EDGE_CURVE('',#2069,#2072,#1303,.T.);
#2536=EDGE_CURVE('',#2070,#2073,#1304,.T.);
#2537=EDGE_CURVE('',#2073,#2074,#1305,.T.);
#2538=EDGE_CURVE('',#2074,#2071,#1306,.T.);
#2539=EDGE_CURVE('',#2073,#2075,#1307,.T.);
#2540=EDGE_CURVE('',#2075,#2076,#1308,.T.);
#2541=EDGE_CURVE('',#2076,#2074,#1309,.T.);
#2542=EDGE_CURVE('',#2075,#2077,#1310,.T.);
#2543=EDGE_CURVE('',#2077,#2078,#1311,.T.);
#2544=EDGE_CURVE('',#2078,#2076,#1312,.T.);
#2545=EDGE_CURVE('',#2077,#2079,#1313,.T.);
#2546=EDGE_CURVE('',#2079,#2080,#1314,.T.);
#2547=EDGE_CURVE('',#2080,#2078,#1315,.T.);
#2548=EDGE_CURVE('',#2079,#2069,#1316,.T.);
#2549=EDGE_CURVE('',#2072,#2080,#1317,.T.);
#2550=EDGE_CURVE('',#2081,#2082,#219,.T.);
#2551=EDGE_CURVE('',#2083,#2081,#220,.T.);
#2552=EDGE_CURVE('',#2083,#2084,#1318,.T.);
#2553=EDGE_CURVE('',#2084,#2084,#1785,.T.);
#2554=EDGE_CURVE('',#2085,#2083,#221,.T.);
#2555=EDGE_CURVE('',#2086,#2085,#222,.T.);
#2556=EDGE_CURVE('',#2087,#2086,#223,.T.);
#2557=EDGE_CURVE('',#2082,#2087,#224,.T.);
#2558=EDGE_CURVE('',#2088,#2088,#1786,.T.);
#2559=EDGE_CURVE('',#2088,#2089,#1319,.T.);
#2560=EDGE_CURVE('',#2090,#2089,#225,.T.);
#2561=EDGE_CURVE('',#2091,#2090,#226,.T.);
#2562=EDGE_CURVE('',#2092,#2091,#227,.T.);
#2563=EDGE_CURVE('',#2093,#2092,#228,.T.);
#2564=EDGE_CURVE('',#2094,#2093,#229,.T.);
#2565=EDGE_CURVE('',#2089,#2094,#230,.T.);
#2566=EDGE_CURVE('',#2085,#2094,#1320,.T.);
#2567=EDGE_CURVE('',#2086,#2093,#1321,.T.);
#2568=EDGE_CURVE('',#2083,#2089,#1322,.T.);
#2569=EDGE_CURVE('',#2081,#2090,#1323,.T.);
#2570=EDGE_CURVE('',#2095,#2095,#1787,.F.);
#2571=EDGE_CURVE('',#2095,#2096,#1324,.T.);
#2572=EDGE_CURVE('',#2096,#2096,#1788,.F.);
#2573=EDGE_CURVE('',#2082,#2091,#1325,.T.);
#2574=EDGE_CURVE('',#2087,#2092,#1326,.T.);
#2575=EDGE_CURVE('',#2097,#2097,#1789,.T.);
#2576=EDGE_CURVE('',#2097,#2098,#1327,.T.);
#2577=EDGE_CURVE('',#2098,#2098,#1790,.T.);
#2578=EDGE_CURVE('',#2099,#2100,#1328,.T.);
#2579=EDGE_CURVE('',#2100,#2101,#1329,.T.);
#2580=EDGE_CURVE('',#2102,#2101,#1330,.T.);
#2581=EDGE_CURVE('',#2099,#2102,#1331,.T.);
#2582=EDGE_CURVE('',#2103,#2099,#1332,.T.);
#2583=EDGE_CURVE('',#2104,#2102,#1333,.T.);
#2584=EDGE_CURVE('',#2103,#2104,#1334,.T.);
#2585=EDGE_CURVE('',#2105,#2103,#1335,.T.);
#2586=EDGE_CURVE('',#2106,#2104,#1336,.T.);
#2587=EDGE_CURVE('',#2105,#2106,#1337,.T.);
#2588=EDGE_CURVE('',#2100,#2105,#1338,.T.);
#2589=EDGE_CURVE('',#2101,#2106,#1339,.T.);
#2590=ORIENTED_EDGE('',*,*,#2107,.F.);
#2591=ORIENTED_EDGE('',*,*,#2108,.T.);
#2592=ORIENTED_EDGE('',*,*,#2109,.F.);
#2593=ORIENTED_EDGE('',*,*,#2108,.F.);
#2594=ORIENTED_EDGE('',*,*,#2110,.F.);
#2595=ORIENTED_EDGE('',*,*,#2111,.T.);
#2596=ORIENTED_EDGE('',*,*,#2112,.F.);
#2597=ORIENTED_EDGE('',*,*,#2111,.F.);
#2598=ORIENTED_EDGE('',*,*,#2113,.T.);
#2599=ORIENTED_EDGE('',*,*,#2114,.T.);
#2600=ORIENTED_EDGE('',*,*,#2115,.F.);
#2601=ORIENTED_EDGE('',*,*,#2116,.F.);
#2602=ORIENTED_EDGE('',*,*,#2109,.T.);
#2603=ORIENTED_EDGE('',*,*,#2112,.T.);
#2604=ORIENTED_EDGE('',*,*,#2117,.T.);
#2605=ORIENTED_EDGE('',*,*,#2116,.T.);
#2606=ORIENTED_EDGE('',*,*,#2118,.F.);
#2607=ORIENTED_EDGE('',*,*,#2119,.F.);
#2608=ORIENTED_EDGE('',*,*,#2120,.T.);
#2609=ORIENTED_EDGE('',*,*,#2119,.T.);
#2610=ORIENTED_EDGE('',*,*,#2121,.F.);
#2611=ORIENTED_EDGE('',*,*,#2122,.F.);
#2612=ORIENTED_EDGE('',*,*,#2107,.T.);
#2613=ORIENTED_EDGE('',*,*,#2110,.T.);
#2614=ORIENTED_EDGE('',*,*,#2123,.T.);
#2615=ORIENTED_EDGE('',*,*,#2122,.T.);
#2616=ORIENTED_EDGE('',*,*,#2124,.F.);
#2617=ORIENTED_EDGE('',*,*,#2114,.F.);
#2618=ORIENTED_EDGE('',*,*,#2124,.T.);
#2619=ORIENTED_EDGE('',*,*,#2121,.T.);
#2620=ORIENTED_EDGE('',*,*,#2118,.T.);
#2621=ORIENTED_EDGE('',*,*,#2115,.T.);
#2622=ORIENTED_EDGE('',*,*,#2123,.F.);
#2623=ORIENTED_EDGE('',*,*,#2113,.F.);
#2624=ORIENTED_EDGE('',*,*,#2117,.F.);
#2625=ORIENTED_EDGE('',*,*,#2120,.F.);
#2626=ORIENTED_EDGE('',*,*,#2125,.F.);
#2627=ORIENTED_EDGE('',*,*,#2126,.T.);
#2628=ORIENTED_EDGE('',*,*,#2127,.F.);
#2629=ORIENTED_EDGE('',*,*,#2128,.F.);
#2630=ORIENTED_EDGE('',*,*,#2129,.F.);
#2631=ORIENTED_EDGE('',*,*,#2130,.T.);
#2632=ORIENTED_EDGE('',*,*,#2131,.F.);
#2633=ORIENTED_EDGE('',*,*,#2126,.F.);
#2634=ORIENTED_EDGE('',*,*,#2132,.F.);
#2635=ORIENTED_EDGE('',*,*,#2133,.T.);
#2636=ORIENTED_EDGE('',*,*,#2134,.F.);
#2637=ORIENTED_EDGE('',*,*,#2130,.F.);
#2638=ORIENTED_EDGE('',*,*,#2135,.F.);
#2639=ORIENTED_EDGE('',*,*,#2136,.T.);
#2640=ORIENTED_EDGE('',*,*,#2137,.F.);
#2641=ORIENTED_EDGE('',*,*,#2133,.F.);
#2642=ORIENTED_EDGE('',*,*,#2138,.F.);
#2643=ORIENTED_EDGE('',*,*,#2139,.T.);
#2644=ORIENTED_EDGE('',*,*,#2140,.F.);
#2645=ORIENTED_EDGE('',*,*,#2136,.F.);
#2646=ORIENTED_EDGE('',*,*,#2141,.F.);
#2647=ORIENTED_EDGE('',*,*,#2142,.T.);
#2648=ORIENTED_EDGE('',*,*,#2143,.F.);
#2649=ORIENTED_EDGE('',*,*,#2139,.F.);
#2650=ORIENTED_EDGE('',*,*,#2144,.F.);
#2651=ORIENTED_EDGE('',*,*,#2145,.T.);
#2652=ORIENTED_EDGE('',*,*,#2146,.F.);
#2653=ORIENTED_EDGE('',*,*,#2142,.F.);
#2654=ORIENTED_EDGE('',*,*,#2147,.F.);
#2655=ORIENTED_EDGE('',*,*,#2148,.T.);
#2656=ORIENTED_EDGE('',*,*,#2149,.F.);
#2657=ORIENTED_EDGE('',*,*,#2145,.F.);
#2658=ORIENTED_EDGE('',*,*,#2150,.F.);
#2659=ORIENTED_EDGE('',*,*,#2151,.F.);
#2660=ORIENTED_EDGE('',*,*,#2152,.F.);
#2661=ORIENTED_EDGE('',*,*,#2148,.F.);
#2662=ORIENTED_EDGE('',*,*,#2153,.F.);
#2663=ORIENTED_EDGE('',*,*,#2154,.T.);
#2664=ORIENTED_EDGE('',*,*,#2155,.F.);
#2665=ORIENTED_EDGE('',*,*,#2156,.F.);
#2666=ORIENTED_EDGE('',*,*,#2157,.F.);
#2667=ORIENTED_EDGE('',*,*,#2158,.T.);
#2668=ORIENTED_EDGE('',*,*,#2159,.F.);
#2669=ORIENTED_EDGE('',*,*,#2154,.F.);
#2670=ORIENTED_EDGE('',*,*,#2160,.F.);
#2671=ORIENTED_EDGE('',*,*,#2161,.T.);
#2672=ORIENTED_EDGE('',*,*,#2162,.F.);
#2673=ORIENTED_EDGE('',*,*,#2158,.F.);
#2674=ORIENTED_EDGE('',*,*,#2163,.F.);
#2675=ORIENTED_EDGE('',*,*,#2164,.T.);
#2676=ORIENTED_EDGE('',*,*,#2165,.F.);
#2677=ORIENTED_EDGE('',*,*,#2161,.F.);
#2678=ORIENTED_EDGE('',*,*,#2166,.F.);
#2679=ORIENTED_EDGE('',*,*,#2167,.T.);
#2680=ORIENTED_EDGE('',*,*,#2168,.F.);
#2681=ORIENTED_EDGE('',*,*,#2164,.F.);
#2682=ORIENTED_EDGE('',*,*,#2169,.F.);
#2683=ORIENTED_EDGE('',*,*,#2170,.T.);
#2684=ORIENTED_EDGE('',*,*,#2171,.F.);
#2685=ORIENTED_EDGE('',*,*,#2167,.F.);
#2686=ORIENTED_EDGE('',*,*,#2172,.F.);
#2687=ORIENTED_EDGE('',*,*,#2173,.T.);
#2688=ORIENTED_EDGE('',*,*,#2174,.F.);
#2689=ORIENTED_EDGE('',*,*,#2170,.F.);
#2690=ORIENTED_EDGE('',*,*,#2175,.F.);
#2691=ORIENTED_EDGE('',*,*,#2176,.T.);
#2692=ORIENTED_EDGE('',*,*,#2177,.F.);
#2693=ORIENTED_EDGE('',*,*,#2173,.F.);
#2694=ORIENTED_EDGE('',*,*,#2178,.F.);
#2695=ORIENTED_EDGE('',*,*,#2179,.F.);
#2696=ORIENTED_EDGE('',*,*,#2180,.F.);
#2697=ORIENTED_EDGE('',*,*,#2176,.F.);
#2698=ORIENTED_EDGE('',*,*,#2181,.F.);
#2699=ORIENTED_EDGE('',*,*,#2182,.T.);
#2700=ORIENTED_EDGE('',*,*,#2183,.F.);
#2701=ORIENTED_EDGE('',*,*,#2184,.F.);
#2702=ORIENTED_EDGE('',*,*,#2185,.F.);
#2703=ORIENTED_EDGE('',*,*,#2186,.T.);
#2704=ORIENTED_EDGE('',*,*,#2187,.F.);
#2705=ORIENTED_EDGE('',*,*,#2182,.F.);
#2706=ORIENTED_EDGE('',*,*,#2188,.F.);
#2707=ORIENTED_EDGE('',*,*,#2189,.T.);
#2708=ORIENTED_EDGE('',*,*,#2190,.F.);
#2709=ORIENTED_EDGE('',*,*,#2186,.F.);
#2710=ORIENTED_EDGE('',*,*,#2191,.F.);
#2711=ORIENTED_EDGE('',*,*,#2192,.T.);
#2712=ORIENTED_EDGE('',*,*,#2193,.F.);
#2713=ORIENTED_EDGE('',*,*,#2189,.F.);
#2714=ORIENTED_EDGE('',*,*,#2194,.F.);
#2715=ORIENTED_EDGE('',*,*,#2195,.T.);
#2716=ORIENTED_EDGE('',*,*,#2196,.F.);
#2717=ORIENTED_EDGE('',*,*,#2192,.F.);
#2718=ORIENTED_EDGE('',*,*,#2197,.F.);
#2719=ORIENTED_EDGE('',*,*,#2198,.T.);
#2720=ORIENTED_EDGE('',*,*,#2199,.F.);
#2721=ORIENTED_EDGE('',*,*,#2195,.F.);
#2722=ORIENTED_EDGE('',*,*,#2200,.F.);
#2723=ORIENTED_EDGE('',*,*,#2201,.T.);
#2724=ORIENTED_EDGE('',*,*,#2202,.F.);
#2725=ORIENTED_EDGE('',*,*,#2198,.F.);
#2726=ORIENTED_EDGE('',*,*,#2203,.F.);
#2727=ORIENTED_EDGE('',*,*,#2204,.T.);
#2728=ORIENTED_EDGE('',*,*,#2205,.F.);
#2729=ORIENTED_EDGE('',*,*,#2201,.F.);
#2730=ORIENTED_EDGE('',*,*,#2206,.F.);
#2731=ORIENTED_EDGE('',*,*,#2207,.F.);
#2732=ORIENTED_EDGE('',*,*,#2208,.F.);
#2733=ORIENTED_EDGE('',*,*,#2204,.F.);
#2734=ORIENTED_EDGE('',*,*,#2209,.F.);
#2735=ORIENTED_EDGE('',*,*,#2210,.T.);
#2736=ORIENTED_EDGE('',*,*,#2211,.F.);
#2737=ORIENTED_EDGE('',*,*,#2212,.F.);
#2738=ORIENTED_EDGE('',*,*,#2213,.F.);
#2739=ORIENTED_EDGE('',*,*,#2214,.T.);
#2740=ORIENTED_EDGE('',*,*,#2215,.F.);
#2741=ORIENTED_EDGE('',*,*,#2210,.F.);
#2742=ORIENTED_EDGE('',*,*,#2216,.F.);
#2743=ORIENTED_EDGE('',*,*,#2217,.T.);
#2744=ORIENTED_EDGE('',*,*,#2218,.F.);
#2745=ORIENTED_EDGE('',*,*,#2214,.F.);
#2746=ORIENTED_EDGE('',*,*,#2219,.F.);
#2747=ORIENTED_EDGE('',*,*,#2220,.T.);
#2748=ORIENTED_EDGE('',*,*,#2221,.F.);
#2749=ORIENTED_EDGE('',*,*,#2217,.F.);
#2750=ORIENTED_EDGE('',*,*,#2222,.F.);
#2751=ORIENTED_EDGE('',*,*,#2223,.T.);
#2752=ORIENTED_EDGE('',*,*,#2224,.F.);
#2753=ORIENTED_EDGE('',*,*,#2220,.F.);
#2754=ORIENTED_EDGE('',*,*,#2225,.F.);
#2755=ORIENTED_EDGE('',*,*,#2226,.T.);
#2756=ORIENTED_EDGE('',*,*,#2227,.F.);
#2757=ORIENTED_EDGE('',*,*,#2223,.F.);
#2758=ORIENTED_EDGE('',*,*,#2228,.F.);
#2759=ORIENTED_EDGE('',*,*,#2229,.T.);
#2760=ORIENTED_EDGE('',*,*,#2230,.F.);
#2761=ORIENTED_EDGE('',*,*,#2226,.F.);
#2762=ORIENTED_EDGE('',*,*,#2231,.F.);
#2763=ORIENTED_EDGE('',*,*,#2232,.T.);
#2764=ORIENTED_EDGE('',*,*,#2233,.F.);
#2765=ORIENTED_EDGE('',*,*,#2229,.F.);
#2766=ORIENTED_EDGE('',*,*,#2234,.F.);
#2767=ORIENTED_EDGE('',*,*,#2235,.F.);
#2768=ORIENTED_EDGE('',*,*,#2236,.F.);
#2769=ORIENTED_EDGE('',*,*,#2232,.F.);
#2770=ORIENTED_EDGE('',*,*,#2237,.F.);
#2771=ORIENTED_EDGE('',*,*,#2238,.T.);
#2772=ORIENTED_EDGE('',*,*,#2239,.F.);
#2773=ORIENTED_EDGE('',*,*,#2238,.F.);
#2774=ORIENTED_EDGE('',*,*,#2151,.T.);
#2775=ORIENTED_EDGE('',*,*,#2240,.T.);
#2776=ORIENTED_EDGE('',*,*,#2241,.T.);
#2777=ORIENTED_EDGE('',*,*,#2242,.F.);
#2778=ORIENTED_EDGE('',*,*,#2128,.T.);
#2779=ORIENTED_EDGE('',*,*,#2243,.F.);
#2780=ORIENTED_EDGE('',*,*,#2244,.F.);
#2781=ORIENTED_EDGE('',*,*,#2245,.T.);
#2782=ORIENTED_EDGE('',*,*,#2179,.T.);
#2783=ORIENTED_EDGE('',*,*,#2246,.T.);
#2784=ORIENTED_EDGE('',*,*,#2244,.T.);
#2785=ORIENTED_EDGE('',*,*,#2247,.F.);
#2786=ORIENTED_EDGE('',*,*,#2156,.T.);
#2787=ORIENTED_EDGE('',*,*,#2248,.F.);
#2788=ORIENTED_EDGE('',*,*,#2249,.F.);
#2789=ORIENTED_EDGE('',*,*,#2250,.T.);
#2790=ORIENTED_EDGE('',*,*,#2207,.T.);
#2791=ORIENTED_EDGE('',*,*,#2251,.T.);
#2792=ORIENTED_EDGE('',*,*,#2249,.T.);
#2793=ORIENTED_EDGE('',*,*,#2252,.F.);
#2794=ORIENTED_EDGE('',*,*,#2184,.T.);
#2795=ORIENTED_EDGE('',*,*,#2253,.F.);
#2796=ORIENTED_EDGE('',*,*,#2254,.F.);
#2797=ORIENTED_EDGE('',*,*,#2255,.T.);
#2798=ORIENTED_EDGE('',*,*,#2235,.T.);
#2799=ORIENTED_EDGE('',*,*,#2256,.T.);
#2800=ORIENTED_EDGE('',*,*,#2254,.T.);
#2801=ORIENTED_EDGE('',*,*,#2257,.F.);
#2802=ORIENTED_EDGE('',*,*,#2212,.T.);
#2803=ORIENTED_EDGE('',*,*,#2258,.F.);
#2804=ORIENTED_EDGE('',*,*,#2241,.F.);
#2805=ORIENTED_EDGE('',*,*,#2259,.T.);
#2806=ORIENTED_EDGE('',*,*,#2127,.T.);
#2807=ORIENTED_EDGE('',*,*,#2131,.T.);
#2808=ORIENTED_EDGE('',*,*,#2134,.T.);
#2809=ORIENTED_EDGE('',*,*,#2137,.T.);
#2810=ORIENTED_EDGE('',*,*,#2140,.T.);
#2811=ORIENTED_EDGE('',*,*,#2143,.T.);
#2812=ORIENTED_EDGE('',*,*,#2146,.T.);
#2813=ORIENTED_EDGE('',*,*,#2149,.T.);
#2814=ORIENTED_EDGE('',*,*,#2152,.T.);
#2815=ORIENTED_EDGE('',*,*,#2242,.T.);
#2816=ORIENTED_EDGE('',*,*,#2258,.T.);
#2817=ORIENTED_EDGE('',*,*,#2211,.T.);
#2818=ORIENTED_EDGE('',*,*,#2215,.T.);
#2819=ORIENTED_EDGE('',*,*,#2218,.T.);
#2820=ORIENTED_EDGE('',*,*,#2221,.T.);
#2821=ORIENTED_EDGE('',*,*,#2224,.T.);
#2822=ORIENTED_EDGE('',*,*,#2227,.T.);
#2823=ORIENTED_EDGE('',*,*,#2230,.T.);
#2824=ORIENTED_EDGE('',*,*,#2233,.T.);
#2825=ORIENTED_EDGE('',*,*,#2236,.T.);
#2826=ORIENTED_EDGE('',*,*,#2257,.T.);
#2827=ORIENTED_EDGE('',*,*,#2253,.T.);
#2828=ORIENTED_EDGE('',*,*,#2183,.T.);
#2829=ORIENTED_EDGE('',*,*,#2187,.T.);
#2830=ORIENTED_EDGE('',*,*,#2190,.T.);
#2831=ORIENTED_EDGE('',*,*,#2193,.T.);
#2832=ORIENTED_EDGE('',*,*,#2196,.T.);
#2833=ORIENTED_EDGE('',*,*,#2199,.T.);
#2834=ORIENTED_EDGE('',*,*,#2202,.T.);
#2835=ORIENTED_EDGE('',*,*,#2205,.T.);
#2836=ORIENTED_EDGE('',*,*,#2208,.T.);
#2837=ORIENTED_EDGE('',*,*,#2252,.T.);
#2838=ORIENTED_EDGE('',*,*,#2248,.T.);
#2839=ORIENTED_EDGE('',*,*,#2155,.T.);
#2840=ORIENTED_EDGE('',*,*,#2159,.T.);
#2841=ORIENTED_EDGE('',*,*,#2162,.T.);
#2842=ORIENTED_EDGE('',*,*,#2165,.T.);
#2843=ORIENTED_EDGE('',*,*,#2168,.T.);
#2844=ORIENTED_EDGE('',*,*,#2171,.T.);
#2845=ORIENTED_EDGE('',*,*,#2174,.T.);
#2846=ORIENTED_EDGE('',*,*,#2177,.T.);
#2847=ORIENTED_EDGE('',*,*,#2180,.T.);
#2848=ORIENTED_EDGE('',*,*,#2247,.T.);
#2849=ORIENTED_EDGE('',*,*,#2243,.T.);
#2850=ORIENTED_EDGE('',*,*,#2239,.T.);
#2851=ORIENTED_EDGE('',*,*,#2125,.T.);
#2852=ORIENTED_EDGE('',*,*,#2245,.F.);
#2853=ORIENTED_EDGE('',*,*,#2246,.F.);
#2854=ORIENTED_EDGE('',*,*,#2178,.T.);
#2855=ORIENTED_EDGE('',*,*,#2175,.T.);
#2856=ORIENTED_EDGE('',*,*,#2172,.T.);
#2857=ORIENTED_EDGE('',*,*,#2169,.T.);
#2858=ORIENTED_EDGE('',*,*,#2166,.T.);
#2859=ORIENTED_EDGE('',*,*,#2163,.T.);
#2860=ORIENTED_EDGE('',*,*,#2160,.T.);
#2861=ORIENTED_EDGE('',*,*,#2157,.T.);
#2862=ORIENTED_EDGE('',*,*,#2153,.T.);
#2863=ORIENTED_EDGE('',*,*,#2250,.F.);
#2864=ORIENTED_EDGE('',*,*,#2251,.F.);
#2865=ORIENTED_EDGE('',*,*,#2206,.T.);
#2866=ORIENTED_EDGE('',*,*,#2203,.T.);
#2867=ORIENTED_EDGE('',*,*,#2200,.T.);
#2868=ORIENTED_EDGE('',*,*,#2197,.T.);
#2869=ORIENTED_EDGE('',*,*,#2194,.T.);
#2870=ORIENTED_EDGE('',*,*,#2191,.T.);
#2871=ORIENTED_EDGE('',*,*,#2188,.T.);
#2872=ORIENTED_EDGE('',*,*,#2185,.T.);
#2873=ORIENTED_EDGE('',*,*,#2181,.T.);
#2874=ORIENTED_EDGE('',*,*,#2255,.F.);
#2875=ORIENTED_EDGE('',*,*,#2256,.F.);
#2876=ORIENTED_EDGE('',*,*,#2234,.T.);
#2877=ORIENTED_EDGE('',*,*,#2231,.T.);
#2878=ORIENTED_EDGE('',*,*,#2228,.T.);
#2879=ORIENTED_EDGE('',*,*,#2225,.T.);
#2880=ORIENTED_EDGE('',*,*,#2222,.T.);
#2881=ORIENTED_EDGE('',*,*,#2219,.T.);
#2882=ORIENTED_EDGE('',*,*,#2216,.T.);
#2883=ORIENTED_EDGE('',*,*,#2213,.T.);
#2884=ORIENTED_EDGE('',*,*,#2209,.T.);
#2885=ORIENTED_EDGE('',*,*,#2259,.F.);
#2886=ORIENTED_EDGE('',*,*,#2240,.F.);
#2887=ORIENTED_EDGE('',*,*,#2150,.T.);
#2888=ORIENTED_EDGE('',*,*,#2147,.T.);
#2889=ORIENTED_EDGE('',*,*,#2144,.T.);
#2890=ORIENTED_EDGE('',*,*,#2141,.T.);
#2891=ORIENTED_EDGE('',*,*,#2138,.T.);
#2892=ORIENTED_EDGE('',*,*,#2135,.T.);
#2893=ORIENTED_EDGE('',*,*,#2132,.T.);
#2894=ORIENTED_EDGE('',*,*,#2129,.T.);
#2895=ORIENTED_EDGE('',*,*,#2237,.T.);
#2896=ORIENTED_EDGE('',*,*,#2260,.F.);
#2897=ORIENTED_EDGE('',*,*,#2261,.T.);
#2898=ORIENTED_EDGE('',*,*,#2262,.F.);
#2899=ORIENTED_EDGE('',*,*,#2261,.F.);
#2900=ORIENTED_EDGE('',*,*,#2263,.F.);
#2901=ORIENTED_EDGE('',*,*,#2264,.T.);
#2902=ORIENTED_EDGE('',*,*,#2265,.F.);
#2903=ORIENTED_EDGE('',*,*,#2264,.F.);
#2904=ORIENTED_EDGE('',*,*,#2266,.F.);
#2905=ORIENTED_EDGE('',*,*,#2267,.T.);
#2906=ORIENTED_EDGE('',*,*,#2268,.F.);
#2907=ORIENTED_EDGE('',*,*,#2267,.F.);
#2908=ORIENTED_EDGE('',*,*,#2269,.F.);
#2909=ORIENTED_EDGE('',*,*,#2270,.T.);
#2910=ORIENTED_EDGE('',*,*,#2271,.F.);
#2911=ORIENTED_EDGE('',*,*,#2270,.F.);
#2912=ORIENTED_EDGE('',*,*,#2272,.F.);
#2913=ORIENTED_EDGE('',*,*,#2273,.F.);
#2914=ORIENTED_EDGE('',*,*,#2274,.T.);
#2915=ORIENTED_EDGE('',*,*,#2275,.T.);
#2916=ORIENTED_EDGE('',*,*,#2276,.F.);
#2917=ORIENTED_EDGE('',*,*,#2277,.T.);
#2918=ORIENTED_EDGE('',*,*,#2274,.F.);
#2919=ORIENTED_EDGE('',*,*,#2278,.F.);
#2920=ORIENTED_EDGE('',*,*,#2279,.T.);
#2921=ORIENTED_EDGE('',*,*,#2272,.T.);
#2922=ORIENTED_EDGE('',*,*,#2280,.T.);
#2923=ORIENTED_EDGE('',*,*,#2281,.T.);
#2924=ORIENTED_EDGE('',*,*,#2282,.F.);
#2925=ORIENTED_EDGE('',*,*,#2283,.F.);
#2926=ORIENTED_EDGE('',*,*,#2284,.T.);
#2927=ORIENTED_EDGE('',*,*,#2285,.T.);
#2928=ORIENTED_EDGE('',*,*,#2260,.T.);
#2929=ORIENTED_EDGE('',*,*,#2263,.T.);
#2930=ORIENTED_EDGE('',*,*,#2286,.F.);
#2931=ORIENTED_EDGE('',*,*,#2287,.F.);
#2932=ORIENTED_EDGE('',*,*,#2281,.F.);
#2933=ORIENTED_EDGE('',*,*,#2288,.T.);
#2934=ORIENTED_EDGE('',*,*,#2288,.F.);
#2935=ORIENTED_EDGE('',*,*,#2280,.F.);
#2936=ORIENTED_EDGE('',*,*,#2275,.F.);
#2937=ORIENTED_EDGE('',*,*,#2277,.F.);
#2938=ORIENTED_EDGE('',*,*,#2289,.F.);
#2939=ORIENTED_EDGE('',*,*,#2269,.T.);
#2940=ORIENTED_EDGE('',*,*,#2290,.T.);
#2941=ORIENTED_EDGE('',*,*,#2291,.T.);
#2942=ORIENTED_EDGE('',*,*,#2292,.T.);
#2943=ORIENTED_EDGE('',*,*,#2293,.T.);
#2944=ORIENTED_EDGE('',*,*,#2294,.F.);
#2945=ORIENTED_EDGE('',*,*,#2286,.T.);
#2946=ORIENTED_EDGE('',*,*,#2289,.T.);
#2947=ORIENTED_EDGE('',*,*,#2276,.T.);
#2948=ORIENTED_EDGE('',*,*,#2290,.F.);
#2949=ORIENTED_EDGE('',*,*,#2278,.T.);
#2950=ORIENTED_EDGE('',*,*,#2273,.T.);
#2951=ORIENTED_EDGE('',*,*,#2279,.F.);
#2952=ORIENTED_EDGE('',*,*,#2295,.T.);
#2953=ORIENTED_EDGE('',*,*,#2268,.T.);
#2954=ORIENTED_EDGE('',*,*,#2291,.F.);
#2955=ORIENTED_EDGE('',*,*,#2295,.F.);
#2956=ORIENTED_EDGE('',*,*,#2285,.F.);
#2957=ORIENTED_EDGE('',*,*,#2296,.T.);
#2958=ORIENTED_EDGE('',*,*,#2284,.F.);
#2959=ORIENTED_EDGE('',*,*,#2297,.F.);
#2960=ORIENTED_EDGE('',*,*,#2298,.F.);
#2961=ORIENTED_EDGE('',*,*,#2292,.F.);
#2962=ORIENTED_EDGE('',*,*,#2296,.F.);
#2963=ORIENTED_EDGE('',*,*,#2266,.T.);
#2964=ORIENTED_EDGE('',*,*,#2298,.T.);
#2965=ORIENTED_EDGE('',*,*,#2299,.T.);
#2966=ORIENTED_EDGE('',*,*,#2300,.F.);
#2967=ORIENTED_EDGE('',*,*,#2293,.F.);
#2968=ORIENTED_EDGE('',*,*,#2262,.T.);
#2969=ORIENTED_EDGE('',*,*,#2265,.T.);
#2970=ORIENTED_EDGE('',*,*,#2297,.T.);
#2971=ORIENTED_EDGE('',*,*,#2283,.T.);
#2972=ORIENTED_EDGE('',*,*,#2301,.F.);
#2973=ORIENTED_EDGE('',*,*,#2299,.F.);
#2974=ORIENTED_EDGE('',*,*,#2294,.T.);
#2975=ORIENTED_EDGE('',*,*,#2300,.T.);
#2976=ORIENTED_EDGE('',*,*,#2301,.T.);
#2977=ORIENTED_EDGE('',*,*,#2282,.T.);
#2978=ORIENTED_EDGE('',*,*,#2287,.T.);
#2979=ORIENTED_EDGE('',*,*,#2271,.T.);
#2980=ORIENTED_EDGE('',*,*,#2302,.F.);
#2981=ORIENTED_EDGE('',*,*,#2303,.T.);
#2982=ORIENTED_EDGE('',*,*,#2304,.F.);
#2983=ORIENTED_EDGE('',*,*,#2303,.F.);
#2984=ORIENTED_EDGE('',*,*,#2305,.F.);
#2985=ORIENTED_EDGE('',*,*,#2306,.F.);
#2986=ORIENTED_EDGE('',*,*,#2307,.F.);
#2987=ORIENTED_EDGE('',*,*,#2308,.F.);
#2988=ORIENTED_EDGE('',*,*,#2309,.T.);
#2989=ORIENTED_EDGE('',*,*,#2307,.T.);
#2990=ORIENTED_EDGE('',*,*,#2309,.F.);
#2991=ORIENTED_EDGE('',*,*,#2310,.F.);
#2992=ORIENTED_EDGE('',*,*,#2311,.T.);
#2993=ORIENTED_EDGE('',*,*,#2308,.T.);
#2994=ORIENTED_EDGE('',*,*,#2311,.F.);
#2995=ORIENTED_EDGE('',*,*,#2310,.T.);
#2996=ORIENTED_EDGE('',*,*,#2312,.F.);
#2997=ORIENTED_EDGE('',*,*,#2313,.F.);
#2998=ORIENTED_EDGE('',*,*,#2314,.T.);
#2999=ORIENTED_EDGE('',*,*,#2306,.T.);
#3000=ORIENTED_EDGE('',*,*,#2315,.T.);
#3001=ORIENTED_EDGE('',*,*,#2312,.T.);
#3002=ORIENTED_EDGE('',*,*,#2315,.F.);
#3003=ORIENTED_EDGE('',*,*,#2305,.T.);
#3004=ORIENTED_EDGE('',*,*,#2302,.T.);
#3005=ORIENTED_EDGE('',*,*,#2314,.F.);
#3006=ORIENTED_EDGE('',*,*,#2304,.T.);
#3007=ORIENTED_EDGE('',*,*,#2316,.F.);
#3008=ORIENTED_EDGE('',*,*,#2317,.T.);
#3009=ORIENTED_EDGE('',*,*,#2313,.T.);
#3010=ORIENTED_EDGE('',*,*,#2317,.F.);
#3011=ORIENTED_EDGE('',*,*,#2316,.T.);
#3012=ORIENTED_EDGE('',*,*,#2318,.F.);
#3013=ORIENTED_EDGE('',*,*,#2319,.T.);
#3014=ORIENTED_EDGE('',*,*,#2320,.T.);
#3015=ORIENTED_EDGE('',*,*,#2319,.F.);
#3016=ORIENTED_EDGE('',*,*,#2321,.F.);
#3017=ORIENTED_EDGE('',*,*,#2322,.T.);
#3018=ORIENTED_EDGE('',*,*,#2323,.T.);
#3019=ORIENTED_EDGE('',*,*,#2322,.F.);
#3020=ORIENTED_EDGE('',*,*,#2321,.T.);
#3021=ORIENTED_EDGE('',*,*,#2318,.T.);
#3022=ORIENTED_EDGE('',*,*,#2323,.F.);
#3023=ORIENTED_EDGE('',*,*,#2320,.F.);
#3024=ORIENTED_EDGE('',*,*,#2324,.F.);
#3025=ORIENTED_EDGE('',*,*,#2325,.T.);
#3026=ORIENTED_EDGE('',*,*,#2324,.T.);
#3027=ORIENTED_EDGE('',*,*,#2325,.F.);
#3028=ORIENTED_EDGE('',*,*,#2326,.F.);
#3029=ORIENTED_EDGE('',*,*,#2327,.F.);
#3030=ORIENTED_EDGE('',*,*,#2328,.T.);
#3031=ORIENTED_EDGE('',*,*,#2329,.F.);
#3032=ORIENTED_EDGE('',*,*,#2329,.T.);
#3033=ORIENTED_EDGE('',*,*,#2330,.T.);
#3034=ORIENTED_EDGE('',*,*,#2331,.F.);
#3035=ORIENTED_EDGE('',*,*,#2332,.F.);
#3036=ORIENTED_EDGE('',*,*,#2328,.F.);
#3037=ORIENTED_EDGE('',*,*,#2332,.T.);
#3038=ORIENTED_EDGE('',*,*,#2333,.F.);
#3039=ORIENTED_EDGE('',*,*,#2334,.T.);
#3040=ORIENTED_EDGE('',*,*,#2327,.T.);
#3041=ORIENTED_EDGE('',*,*,#2326,.T.);
#3042=ORIENTED_EDGE('',*,*,#2334,.F.);
#3043=ORIENTED_EDGE('',*,*,#2335,.F.);
#3044=ORIENTED_EDGE('',*,*,#2330,.F.);
#3045=ORIENTED_EDGE('',*,*,#2335,.T.);
#3046=ORIENTED_EDGE('',*,*,#2333,.T.);
#3047=ORIENTED_EDGE('',*,*,#2331,.T.);
#3048=ORIENTED_EDGE('',*,*,#2336,.T.);
#3049=ORIENTED_EDGE('',*,*,#2337,.T.);
#3050=ORIENTED_EDGE('',*,*,#2338,.T.);
#3051=ORIENTED_EDGE('',*,*,#2339,.T.);
#3052=ORIENTED_EDGE('',*,*,#2340,.T.);
#3053=ORIENTED_EDGE('',*,*,#2341,.T.);
#3054=ORIENTED_EDGE('',*,*,#2340,.F.);
#3055=ORIENTED_EDGE('',*,*,#2342,.F.);
#3056=ORIENTED_EDGE('',*,*,#2343,.T.);
#3057=ORIENTED_EDGE('',*,*,#2344,.F.);
#3058=ORIENTED_EDGE('',*,*,#2343,.F.);
#3059=ORIENTED_EDGE('',*,*,#2345,.F.);
#3060=ORIENTED_EDGE('',*,*,#2346,.F.);
#3061=ORIENTED_EDGE('',*,*,#2347,.F.);
#3062=ORIENTED_EDGE('',*,*,#2339,.F.);
#3063=ORIENTED_EDGE('',*,*,#2348,.F.);
#3064=ORIENTED_EDGE('',*,*,#2349,.F.);
#3065=ORIENTED_EDGE('',*,*,#2345,.T.);
#3066=ORIENTED_EDGE('',*,*,#2342,.T.);
#3067=ORIENTED_EDGE('',*,*,#2341,.F.);
#3068=ORIENTED_EDGE('',*,*,#2347,.T.);
#3069=ORIENTED_EDGE('',*,*,#2350,.F.);
#3070=ORIENTED_EDGE('',*,*,#2351,.F.);
#3071=ORIENTED_EDGE('',*,*,#2352,.T.);
#3072=ORIENTED_EDGE('',*,*,#2353,.T.);
#3073=ORIENTED_EDGE('',*,*,#2354,.T.);
#3074=ORIENTED_EDGE('',*,*,#2350,.T.);
#3075=ORIENTED_EDGE('',*,*,#2346,.T.);
#3076=ORIENTED_EDGE('',*,*,#2349,.T.);
#3077=ORIENTED_EDGE('',*,*,#2336,.F.);
#3078=ORIENTED_EDGE('',*,*,#2351,.T.);
#3079=ORIENTED_EDGE('',*,*,#2354,.F.);
#3080=ORIENTED_EDGE('',*,*,#2355,.T.);
#3081=ORIENTED_EDGE('',*,*,#2356,.F.);
#3082=ORIENTED_EDGE('',*,*,#2357,.F.);
#3083=ORIENTED_EDGE('',*,*,#2353,.F.);
#3084=ORIENTED_EDGE('',*,*,#2358,.T.);
#3085=ORIENTED_EDGE('',*,*,#2359,.F.);
#3086=ORIENTED_EDGE('',*,*,#2355,.F.);
#3087=ORIENTED_EDGE('',*,*,#2337,.F.);
#3088=ORIENTED_EDGE('',*,*,#2357,.T.);
#3089=ORIENTED_EDGE('',*,*,#2360,.F.);
#3090=ORIENTED_EDGE('',*,*,#2361,.F.);
#3091=ORIENTED_EDGE('',*,*,#2338,.F.);
#3092=ORIENTED_EDGE('',*,*,#2361,.T.);
#3093=ORIENTED_EDGE('',*,*,#2362,.F.);
#3094=ORIENTED_EDGE('',*,*,#2358,.F.);
#3095=ORIENTED_EDGE('',*,*,#2352,.F.);
#3096=ORIENTED_EDGE('',*,*,#2348,.T.);
#3097=ORIENTED_EDGE('',*,*,#2362,.T.);
#3098=ORIENTED_EDGE('',*,*,#2360,.T.);
#3099=ORIENTED_EDGE('',*,*,#2356,.T.);
#3100=ORIENTED_EDGE('',*,*,#2359,.T.);
#3101=ORIENTED_EDGE('',*,*,#2344,.T.);
#3102=ORIENTED_EDGE('',*,*,#2363,.T.);
#3103=ORIENTED_EDGE('',*,*,#2364,.T.);
#3104=ORIENTED_EDGE('',*,*,#2365,.T.);
#3105=ORIENTED_EDGE('',*,*,#2366,.F.);
#3106=ORIENTED_EDGE('',*,*,#2367,.T.);
#3107=ORIENTED_EDGE('',*,*,#2368,.T.);
#3108=ORIENTED_EDGE('',*,*,#2369,.T.);
#3109=ORIENTED_EDGE('',*,*,#2364,.F.);
#3110=ORIENTED_EDGE('',*,*,#2370,.T.);
#3111=ORIENTED_EDGE('',*,*,#2371,.T.);
#3112=ORIENTED_EDGE('',*,*,#2372,.T.);
#3113=ORIENTED_EDGE('',*,*,#2368,.F.);
#3114=ORIENTED_EDGE('',*,*,#2373,.T.);
#3115=ORIENTED_EDGE('',*,*,#2374,.T.);
#3116=ORIENTED_EDGE('',*,*,#2375,.T.);
#3117=ORIENTED_EDGE('',*,*,#2371,.F.);
#3118=ORIENTED_EDGE('',*,*,#2376,.T.);
#3119=ORIENTED_EDGE('',*,*,#2377,.T.);
#3120=ORIENTED_EDGE('',*,*,#2378,.T.);
#3121=ORIENTED_EDGE('',*,*,#2374,.F.);
#3122=ORIENTED_EDGE('',*,*,#2379,.T.);
#3123=ORIENTED_EDGE('',*,*,#2366,.T.);
#3124=ORIENTED_EDGE('',*,*,#2380,.T.);
#3125=ORIENTED_EDGE('',*,*,#2377,.F.);
#3126=ORIENTED_EDGE('',*,*,#2379,.F.);
#3127=ORIENTED_EDGE('',*,*,#2376,.F.);
#3128=ORIENTED_EDGE('',*,*,#2373,.F.);
#3129=ORIENTED_EDGE('',*,*,#2370,.F.);
#3130=ORIENTED_EDGE('',*,*,#2367,.F.);
#3131=ORIENTED_EDGE('',*,*,#2363,.F.);
#3132=ORIENTED_EDGE('',*,*,#2380,.F.);
#3133=ORIENTED_EDGE('',*,*,#2365,.F.);
#3134=ORIENTED_EDGE('',*,*,#2369,.F.);
#3135=ORIENTED_EDGE('',*,*,#2372,.F.);
#3136=ORIENTED_EDGE('',*,*,#2375,.F.);
#3137=ORIENTED_EDGE('',*,*,#2378,.F.);
#3138=ORIENTED_EDGE('',*,*,#2381,.F.);
#3139=ORIENTED_EDGE('',*,*,#2382,.F.);
#3140=ORIENTED_EDGE('',*,*,#2383,.F.);
#3141=ORIENTED_EDGE('',*,*,#2384,.T.);
#3142=ORIENTED_EDGE('',*,*,#2382,.T.);
#3143=ORIENTED_EDGE('',*,*,#2384,.F.);
#3144=ORIENTED_EDGE('',*,*,#2385,.F.);
#3145=ORIENTED_EDGE('',*,*,#2386,.T.);
#3146=ORIENTED_EDGE('',*,*,#2383,.T.);
#3147=ORIENTED_EDGE('',*,*,#2386,.F.);
#3148=ORIENTED_EDGE('',*,*,#2387,.F.);
#3149=ORIENTED_EDGE('',*,*,#2388,.T.);
#3150=ORIENTED_EDGE('',*,*,#2385,.T.);
#3151=ORIENTED_EDGE('',*,*,#2388,.F.);
#3152=ORIENTED_EDGE('',*,*,#2387,.T.);
#3153=ORIENTED_EDGE('',*,*,#2389,.F.);
#3154=ORIENTED_EDGE('',*,*,#2390,.F.);
#3155=ORIENTED_EDGE('',*,*,#2391,.T.);
#3156=ORIENTED_EDGE('',*,*,#2389,.T.);
#3157=ORIENTED_EDGE('',*,*,#2391,.F.);
#3158=ORIENTED_EDGE('',*,*,#2381,.T.);
#3159=ORIENTED_EDGE('',*,*,#2392,.T.);
#3160=ORIENTED_EDGE('',*,*,#2390,.T.);
#3161=ORIENTED_EDGE('',*,*,#2392,.F.);
#3162=ORIENTED_EDGE('',*,*,#2393,.F.);
#3163=ORIENTED_EDGE('',*,*,#2394,.T.);
#3164=ORIENTED_EDGE('',*,*,#2395,.F.);
#3165=ORIENTED_EDGE('',*,*,#2394,.F.);
#3166=ORIENTED_EDGE('',*,*,#2396,.F.);
#3167=ORIENTED_EDGE('',*,*,#2397,.T.);
#3168=ORIENTED_EDGE('',*,*,#2398,.F.);
#3169=ORIENTED_EDGE('',*,*,#2397,.F.);
#3170=ORIENTED_EDGE('',*,*,#2399,.F.);
#3171=ORIENTED_EDGE('',*,*,#2400,.T.);
#3172=ORIENTED_EDGE('',*,*,#2401,.F.);
#3173=ORIENTED_EDGE('',*,*,#2400,.F.);
#3174=ORIENTED_EDGE('',*,*,#2402,.F.);
#3175=ORIENTED_EDGE('',*,*,#2403,.T.);
#3176=ORIENTED_EDGE('',*,*,#2404,.F.);
#3177=ORIENTED_EDGE('',*,*,#2403,.F.);
#3178=ORIENTED_EDGE('',*,*,#2405,.F.);
#3179=ORIENTED_EDGE('',*,*,#2406,.T.);
#3180=ORIENTED_EDGE('',*,*,#2407,.F.);
#3181=ORIENTED_EDGE('',*,*,#2406,.F.);
#3182=ORIENTED_EDGE('',*,*,#2408,.T.);
#3183=ORIENTED_EDGE('',*,*,#2409,.T.);
#3184=ORIENTED_EDGE('',*,*,#2410,.F.);
#3185=ORIENTED_EDGE('',*,*,#2411,.F.);
#3186=ORIENTED_EDGE('',*,*,#2395,.T.);
#3187=ORIENTED_EDGE('',*,*,#2398,.T.);
#3188=ORIENTED_EDGE('',*,*,#2401,.T.);
#3189=ORIENTED_EDGE('',*,*,#2404,.T.);
#3190=ORIENTED_EDGE('',*,*,#2407,.T.);
#3191=ORIENTED_EDGE('',*,*,#2412,.T.);
#3192=ORIENTED_EDGE('',*,*,#2411,.T.);
#3193=ORIENTED_EDGE('',*,*,#2413,.F.);
#3194=ORIENTED_EDGE('',*,*,#2414,.F.);
#3195=ORIENTED_EDGE('',*,*,#2415,.T.);
#3196=ORIENTED_EDGE('',*,*,#2414,.T.);
#3197=ORIENTED_EDGE('',*,*,#2416,.F.);
#3198=ORIENTED_EDGE('',*,*,#2417,.F.);
#3199=ORIENTED_EDGE('',*,*,#2393,.T.);
#3200=ORIENTED_EDGE('',*,*,#2396,.T.);
#3201=ORIENTED_EDGE('',*,*,#2399,.T.);
#3202=ORIENTED_EDGE('',*,*,#2402,.T.);
#3203=ORIENTED_EDGE('',*,*,#2405,.T.);
#3204=ORIENTED_EDGE('',*,*,#2418,.T.);
#3205=ORIENTED_EDGE('',*,*,#2417,.T.);
#3206=ORIENTED_EDGE('',*,*,#2419,.F.);
#3207=ORIENTED_EDGE('',*,*,#2409,.F.);
#3208=ORIENTED_EDGE('',*,*,#2419,.T.);
#3209=ORIENTED_EDGE('',*,*,#2416,.T.);
#3210=ORIENTED_EDGE('',*,*,#2413,.T.);
#3211=ORIENTED_EDGE('',*,*,#2410,.T.);
#3212=ORIENTED_EDGE('',*,*,#2418,.F.);
#3213=ORIENTED_EDGE('',*,*,#2408,.F.);
#3214=ORIENTED_EDGE('',*,*,#2412,.F.);
#3215=ORIENTED_EDGE('',*,*,#2415,.F.);
#3216=ORIENTED_EDGE('',*,*,#2420,.F.);
#3217=ORIENTED_EDGE('',*,*,#2421,.T.);
#3218=ORIENTED_EDGE('',*,*,#2422,.F.);
#3219=ORIENTED_EDGE('',*,*,#2421,.F.);
#3220=ORIENTED_EDGE('',*,*,#2423,.F.);
#3221=ORIENTED_EDGE('',*,*,#2424,.T.);
#3222=ORIENTED_EDGE('',*,*,#2425,.F.);
#3223=ORIENTED_EDGE('',*,*,#2424,.F.);
#3224=ORIENTED_EDGE('',*,*,#2426,.F.);
#3225=ORIENTED_EDGE('',*,*,#2427,.T.);
#3226=ORIENTED_EDGE('',*,*,#2428,.F.);
#3227=ORIENTED_EDGE('',*,*,#2427,.F.);
#3228=ORIENTED_EDGE('',*,*,#2429,.F.);
#3229=ORIENTED_EDGE('',*,*,#2430,.F.);
#3230=ORIENTED_EDGE('',*,*,#2431,.T.);
#3231=ORIENTED_EDGE('',*,*,#2432,.F.);
#3232=ORIENTED_EDGE('',*,*,#2433,.F.);
#3233=ORIENTED_EDGE('',*,*,#2434,.F.);
#3234=ORIENTED_EDGE('',*,*,#2435,.F.);
#3235=ORIENTED_EDGE('',*,*,#2436,.F.);
#3236=ORIENTED_EDGE('',*,*,#2437,.F.);
#3237=ORIENTED_EDGE('',*,*,#2435,.T.);
#3238=ORIENTED_EDGE('',*,*,#2438,.F.);
#3239=ORIENTED_EDGE('',*,*,#2439,.F.);
#3240=ORIENTED_EDGE('',*,*,#2440,.F.);
#3241=ORIENTED_EDGE('',*,*,#2439,.T.);
#3242=ORIENTED_EDGE('',*,*,#2441,.F.);
#3243=ORIENTED_EDGE('',*,*,#2442,.F.);
#3244=ORIENTED_EDGE('',*,*,#2443,.F.);
#3245=ORIENTED_EDGE('',*,*,#2442,.T.);
#3246=ORIENTED_EDGE('',*,*,#2444,.F.);
#3247=ORIENTED_EDGE('',*,*,#2431,.F.);
#3248=ORIENTED_EDGE('',*,*,#2433,.T.);
#3249=ORIENTED_EDGE('',*,*,#2445,.F.);
#3250=ORIENTED_EDGE('',*,*,#2446,.F.);
#3251=ORIENTED_EDGE('',*,*,#2447,.F.);
#3252=ORIENTED_EDGE('',*,*,#2426,.T.);
#3253=ORIENTED_EDGE('',*,*,#2448,.T.);
#3254=ORIENTED_EDGE('',*,*,#2449,.F.);
#3255=ORIENTED_EDGE('',*,*,#2445,.T.);
#3256=ORIENTED_EDGE('',*,*,#2436,.T.);
#3257=ORIENTED_EDGE('',*,*,#2437,.T.);
#3258=ORIENTED_EDGE('',*,*,#2440,.T.);
#3259=ORIENTED_EDGE('',*,*,#2443,.T.);
#3260=ORIENTED_EDGE('',*,*,#2430,.T.);
#3261=ORIENTED_EDGE('',*,*,#2420,.T.);
#3262=ORIENTED_EDGE('',*,*,#2423,.T.);
#3263=ORIENTED_EDGE('',*,*,#2447,.T.);
#3264=ORIENTED_EDGE('',*,*,#2450,.F.);
#3265=ORIENTED_EDGE('',*,*,#2451,.T.);
#3266=ORIENTED_EDGE('',*,*,#2432,.T.);
#3267=ORIENTED_EDGE('',*,*,#2444,.T.);
#3268=ORIENTED_EDGE('',*,*,#2441,.T.);
#3269=ORIENTED_EDGE('',*,*,#2438,.T.);
#3270=ORIENTED_EDGE('',*,*,#2434,.T.);
#3271=ORIENTED_EDGE('',*,*,#2422,.T.);
#3272=ORIENTED_EDGE('',*,*,#2425,.T.);
#3273=ORIENTED_EDGE('',*,*,#2449,.T.);
#3274=ORIENTED_EDGE('',*,*,#2452,.F.);
#3275=ORIENTED_EDGE('',*,*,#2450,.T.);
#3276=ORIENTED_EDGE('',*,*,#2446,.T.);
#3277=ORIENTED_EDGE('',*,*,#2429,.T.);
#3278=ORIENTED_EDGE('',*,*,#2451,.F.);
#3279=ORIENTED_EDGE('',*,*,#2452,.T.);
#3280=ORIENTED_EDGE('',*,*,#2448,.F.);
#3281=ORIENTED_EDGE('',*,*,#2428,.T.);
#3282=ORIENTED_EDGE('',*,*,#2453,.F.);
#3283=ORIENTED_EDGE('',*,*,#2454,.F.);
#3284=ORIENTED_EDGE('',*,*,#2455,.T.);
#3285=ORIENTED_EDGE('',*,*,#2453,.T.);
#3286=ORIENTED_EDGE('',*,*,#2455,.F.);
#3287=ORIENTED_EDGE('',*,*,#2456,.F.);
#3288=ORIENTED_EDGE('',*,*,#2457,.T.);
#3289=ORIENTED_EDGE('',*,*,#2454,.T.);
#3290=ORIENTED_EDGE('',*,*,#2457,.F.);
#3291=ORIENTED_EDGE('',*,*,#2458,.F.);
#3292=ORIENTED_EDGE('',*,*,#2459,.T.);
#3293=ORIENTED_EDGE('',*,*,#2456,.T.);
#3294=ORIENTED_EDGE('',*,*,#2459,.F.);
#3295=ORIENTED_EDGE('',*,*,#2458,.T.);
#3296=ORIENTED_EDGE('',*,*,#2460,.F.);
#3297=ORIENTED_EDGE('',*,*,#2461,.F.);
#3298=ORIENTED_EDGE('',*,*,#2462,.T.);
#3299=ORIENTED_EDGE('',*,*,#2460,.T.);
#3300=ORIENTED_EDGE('',*,*,#2462,.F.);
#3301=ORIENTED_EDGE('',*,*,#2463,.F.);
#3302=ORIENTED_EDGE('',*,*,#2464,.T.);
#3303=ORIENTED_EDGE('',*,*,#2461,.T.);
#3304=ORIENTED_EDGE('',*,*,#2464,.F.);
#3305=ORIENTED_EDGE('',*,*,#2465,.F.);
#3306=ORIENTED_EDGE('',*,*,#2466,.T.);
#3307=ORIENTED_EDGE('',*,*,#2463,.T.);
#3308=ORIENTED_EDGE('',*,*,#2466,.F.);
#3309=ORIENTED_EDGE('',*,*,#2465,.T.);
#3310=ORIENTED_EDGE('',*,*,#2467,.T.);
#3311=ORIENTED_EDGE('',*,*,#2468,.T.);
#3312=ORIENTED_EDGE('',*,*,#2469,.T.);
#3313=ORIENTED_EDGE('',*,*,#2470,.F.);
#3314=ORIENTED_EDGE('',*,*,#2471,.T.);
#3315=ORIENTED_EDGE('',*,*,#2472,.T.);
#3316=ORIENTED_EDGE('',*,*,#2473,.T.);
#3317=ORIENTED_EDGE('',*,*,#2468,.F.);
#3318=ORIENTED_EDGE('',*,*,#2474,.T.);
#3319=ORIENTED_EDGE('',*,*,#2475,.T.);
#3320=ORIENTED_EDGE('',*,*,#2476,.T.);
#3321=ORIENTED_EDGE('',*,*,#2472,.F.);
#3322=ORIENTED_EDGE('',*,*,#2477,.T.);
#3323=ORIENTED_EDGE('',*,*,#2478,.T.);
#3324=ORIENTED_EDGE('',*,*,#2479,.T.);
#3325=ORIENTED_EDGE('',*,*,#2475,.F.);
#3326=ORIENTED_EDGE('',*,*,#2480,.T.);
#3327=ORIENTED_EDGE('',*,*,#2481,.T.);
#3328=ORIENTED_EDGE('',*,*,#2482,.T.);
#3329=ORIENTED_EDGE('',*,*,#2478,.F.);
#3330=ORIENTED_EDGE('',*,*,#2483,.T.);
#3331=ORIENTED_EDGE('',*,*,#2470,.T.);
#3332=ORIENTED_EDGE('',*,*,#2484,.T.);
#3333=ORIENTED_EDGE('',*,*,#2481,.F.);
#3334=ORIENTED_EDGE('',*,*,#2483,.F.);
#3335=ORIENTED_EDGE('',*,*,#2480,.F.);
#3336=ORIENTED_EDGE('',*,*,#2477,.F.);
#3337=ORIENTED_EDGE('',*,*,#2474,.F.);
#3338=ORIENTED_EDGE('',*,*,#2471,.F.);
#3339=ORIENTED_EDGE('',*,*,#2467,.F.);
#3340=ORIENTED_EDGE('',*,*,#2484,.F.);
#3341=ORIENTED_EDGE('',*,*,#2469,.F.);
#3342=ORIENTED_EDGE('',*,*,#2473,.F.);
#3343=ORIENTED_EDGE('',*,*,#2476,.F.);
#3344=ORIENTED_EDGE('',*,*,#2479,.F.);
#3345=ORIENTED_EDGE('',*,*,#2482,.F.);
#3346=ORIENTED_EDGE('',*,*,#2485,.F.);
#3347=ORIENTED_EDGE('',*,*,#2486,.F.);
#3348=ORIENTED_EDGE('',*,*,#2487,.T.);
#3349=ORIENTED_EDGE('',*,*,#2488,.F.);
#3350=ORIENTED_EDGE('',*,*,#2487,.F.);
#3351=ORIENTED_EDGE('',*,*,#2489,.F.);
#3352=ORIENTED_EDGE('',*,*,#2490,.F.);
#3353=ORIENTED_EDGE('',*,*,#2491,.F.);
#3354=ORIENTED_EDGE('',*,*,#2492,.F.);
#3355=ORIENTED_EDGE('',*,*,#2493,.F.);
#3356=ORIENTED_EDGE('',*,*,#2494,.T.);
#3357=ORIENTED_EDGE('',*,*,#2495,.F.);
#3358=ORIENTED_EDGE('',*,*,#2496,.F.);
#3359=ORIENTED_EDGE('',*,*,#2497,.F.);
#3360=ORIENTED_EDGE('',*,*,#2498,.F.);
#3361=ORIENTED_EDGE('',*,*,#2499,.F.);
#3362=ORIENTED_EDGE('',*,*,#2500,.F.);
#3363=ORIENTED_EDGE('',*,*,#2494,.F.);
#3364=ORIENTED_EDGE('',*,*,#2490,.T.);
#3365=ORIENTED_EDGE('',*,*,#2501,.T.);
#3366=ORIENTED_EDGE('',*,*,#2499,.T.);
#3367=ORIENTED_EDGE('',*,*,#2502,.F.);
#3368=ORIENTED_EDGE('',*,*,#2489,.T.);
#3369=ORIENTED_EDGE('',*,*,#2503,.T.);
#3370=ORIENTED_EDGE('',*,*,#2500,.T.);
#3371=ORIENTED_EDGE('',*,*,#2501,.F.);
#3372=ORIENTED_EDGE('',*,*,#2486,.T.);
#3373=ORIENTED_EDGE('',*,*,#2504,.T.);
#3374=ORIENTED_EDGE('',*,*,#2495,.T.);
#3375=ORIENTED_EDGE('',*,*,#2503,.F.);
#3376=ORIENTED_EDGE('',*,*,#2505,.F.);
#3377=ORIENTED_EDGE('',*,*,#2506,.T.);
#3378=ORIENTED_EDGE('',*,*,#2507,.T.);
#3379=ORIENTED_EDGE('',*,*,#2506,.F.);
#3380=ORIENTED_EDGE('',*,*,#2485,.T.);
#3381=ORIENTED_EDGE('',*,*,#2508,.T.);
#3382=ORIENTED_EDGE('',*,*,#2496,.T.);
#3383=ORIENTED_EDGE('',*,*,#2504,.F.);
#3384=ORIENTED_EDGE('',*,*,#2491,.T.);
#3385=ORIENTED_EDGE('',*,*,#2502,.T.);
#3386=ORIENTED_EDGE('',*,*,#2498,.T.);
#3387=ORIENTED_EDGE('',*,*,#2509,.F.);
#3388=ORIENTED_EDGE('',*,*,#2492,.T.);
#3389=ORIENTED_EDGE('',*,*,#2509,.T.);
#3390=ORIENTED_EDGE('',*,*,#2497,.T.);
#3391=ORIENTED_EDGE('',*,*,#2508,.F.);
#3392=ORIENTED_EDGE('',*,*,#2493,.T.);
#3393=ORIENTED_EDGE('',*,*,#2505,.T.);
#3394=ORIENTED_EDGE('',*,*,#2488,.T.);
#3395=ORIENTED_EDGE('',*,*,#2507,.F.);
#3396=ORIENTED_EDGE('',*,*,#2510,.T.);
#3397=ORIENTED_EDGE('',*,*,#2511,.T.);
#3398=ORIENTED_EDGE('',*,*,#2512,.T.);
#3399=ORIENTED_EDGE('',*,*,#2511,.F.);
#3400=ORIENTED_EDGE('',*,*,#2512,.F.);
#3401=ORIENTED_EDGE('',*,*,#2513,.T.);
#3402=ORIENTED_EDGE('',*,*,#2514,.T.);
#3403=ORIENTED_EDGE('',*,*,#2513,.F.);
#3404=ORIENTED_EDGE('',*,*,#2515,.T.);
#3405=ORIENTED_EDGE('',*,*,#2510,.F.);
#3406=ORIENTED_EDGE('',*,*,#2515,.F.);
#3407=ORIENTED_EDGE('',*,*,#2516,.T.);
#3408=ORIENTED_EDGE('',*,*,#2517,.T.);
#3409=ORIENTED_EDGE('',*,*,#2516,.F.);
#3410=ORIENTED_EDGE('',*,*,#2517,.F.);
#3411=ORIENTED_EDGE('',*,*,#2514,.F.);
#3412=ORIENTED_EDGE('',*,*,#2518,.F.);
#3413=ORIENTED_EDGE('',*,*,#2519,.F.);
#3414=ORIENTED_EDGE('',*,*,#2520,.T.);
#3415=ORIENTED_EDGE('',*,*,#2518,.T.);
#3416=ORIENTED_EDGE('',*,*,#2520,.F.);
#3417=ORIENTED_EDGE('',*,*,#2521,.F.);
#3418=ORIENTED_EDGE('',*,*,#2522,.T.);
#3419=ORIENTED_EDGE('',*,*,#2519,.T.);
#3420=ORIENTED_EDGE('',*,*,#2522,.F.);
#3421=ORIENTED_EDGE('',*,*,#2523,.F.);
#3422=ORIENTED_EDGE('',*,*,#2524,.T.);
#3423=ORIENTED_EDGE('',*,*,#2521,.T.);
#3424=ORIENTED_EDGE('',*,*,#2524,.F.);
#3425=ORIENTED_EDGE('',*,*,#2523,.T.);
#3426=ORIENTED_EDGE('',*,*,#2525,.F.);
#3427=ORIENTED_EDGE('',*,*,#2526,.F.);
#3428=ORIENTED_EDGE('',*,*,#2527,.T.);
#3429=ORIENTED_EDGE('',*,*,#2525,.T.);
#3430=ORIENTED_EDGE('',*,*,#2527,.F.);
#3431=ORIENTED_EDGE('',*,*,#2528,.F.);
#3432=ORIENTED_EDGE('',*,*,#2529,.T.);
#3433=ORIENTED_EDGE('',*,*,#2526,.T.);
#3434=ORIENTED_EDGE('',*,*,#2529,.F.);
#3435=ORIENTED_EDGE('',*,*,#2530,.F.);
#3436=ORIENTED_EDGE('',*,*,#2531,.T.);
#3437=ORIENTED_EDGE('',*,*,#2528,.T.);
#3438=ORIENTED_EDGE('',*,*,#2531,.F.);
#3439=ORIENTED_EDGE('',*,*,#2530,.T.);
#3440=ORIENTED_EDGE('',*,*,#2532,.T.);
#3441=ORIENTED_EDGE('',*,*,#2533,.T.);
#3442=ORIENTED_EDGE('',*,*,#2534,.T.);
#3443=ORIENTED_EDGE('',*,*,#2535,.F.);
#3444=ORIENTED_EDGE('',*,*,#2536,.T.);
#3445=ORIENTED_EDGE('',*,*,#2537,.T.);
#3446=ORIENTED_EDGE('',*,*,#2538,.T.);
#3447=ORIENTED_EDGE('',*,*,#2533,.F.);
#3448=ORIENTED_EDGE('',*,*,#2539,.T.);
#3449=ORIENTED_EDGE('',*,*,#2540,.T.);
#3450=ORIENTED_EDGE('',*,*,#2541,.T.);
#3451=ORIENTED_EDGE('',*,*,#2537,.F.);
#3452=ORIENTED_EDGE('',*,*,#2542,.T.);
#3453=ORIENTED_EDGE('',*,*,#2543,.T.);
#3454=ORIENTED_EDGE('',*,*,#2544,.T.);
#3455=ORIENTED_EDGE('',*,*,#2540,.F.);
#3456=ORIENTED_EDGE('',*,*,#2545,.T.);
#3457=ORIENTED_EDGE('',*,*,#2546,.T.);
#3458=ORIENTED_EDGE('',*,*,#2547,.T.);
#3459=ORIENTED_EDGE('',*,*,#2543,.F.);
#3460=ORIENTED_EDGE('',*,*,#2548,.T.);
#3461=ORIENTED_EDGE('',*,*,#2535,.T.);
#3462=ORIENTED_EDGE('',*,*,#2549,.T.);
#3463=ORIENTED_EDGE('',*,*,#2546,.F.);
#3464=ORIENTED_EDGE('',*,*,#2548,.F.);
#3465=ORIENTED_EDGE('',*,*,#2545,.F.);
#3466=ORIENTED_EDGE('',*,*,#2542,.F.);
#3467=ORIENTED_EDGE('',*,*,#2539,.F.);
#3468=ORIENTED_EDGE('',*,*,#2536,.F.);
#3469=ORIENTED_EDGE('',*,*,#2532,.F.);
#3470=ORIENTED_EDGE('',*,*,#2549,.F.);
#3471=ORIENTED_EDGE('',*,*,#2534,.F.);
#3472=ORIENTED_EDGE('',*,*,#2538,.F.);
#3473=ORIENTED_EDGE('',*,*,#2541,.F.);
#3474=ORIENTED_EDGE('',*,*,#2544,.F.);
#3475=ORIENTED_EDGE('',*,*,#2547,.F.);
#3476=ORIENTED_EDGE('',*,*,#2550,.F.);
#3477=ORIENTED_EDGE('',*,*,#2551,.F.);
#3478=ORIENTED_EDGE('',*,*,#2552,.T.);
#3479=ORIENTED_EDGE('',*,*,#2553,.F.);
#3480=ORIENTED_EDGE('',*,*,#2552,.F.);
#3481=ORIENTED_EDGE('',*,*,#2554,.F.);
#3482=ORIENTED_EDGE('',*,*,#2555,.F.);
#3483=ORIENTED_EDGE('',*,*,#2556,.F.);
#3484=ORIENTED_EDGE('',*,*,#2557,.F.);
#3485=ORIENTED_EDGE('',*,*,#2558,.F.);
#3486=ORIENTED_EDGE('',*,*,#2559,.T.);
#3487=ORIENTED_EDGE('',*,*,#2560,.F.);
#3488=ORIENTED_EDGE('',*,*,#2561,.F.);
#3489=ORIENTED_EDGE('',*,*,#2562,.F.);
#3490=ORIENTED_EDGE('',*,*,#2563,.F.);
#3491=ORIENTED_EDGE('',*,*,#2564,.F.);
#3492=ORIENTED_EDGE('',*,*,#2565,.F.);
#3493=ORIENTED_EDGE('',*,*,#2559,.F.);
#3494=ORIENTED_EDGE('',*,*,#2555,.T.);
#3495=ORIENTED_EDGE('',*,*,#2566,.T.);
#3496=ORIENTED_EDGE('',*,*,#2564,.T.);
#3497=ORIENTED_EDGE('',*,*,#2567,.F.);
#3498=ORIENTED_EDGE('',*,*,#2554,.T.);
#3499=ORIENTED_EDGE('',*,*,#2568,.T.);
#3500=ORIENTED_EDGE('',*,*,#2565,.T.);
#3501=ORIENTED_EDGE('',*,*,#2566,.F.);
#3502=ORIENTED_EDGE('',*,*,#2551,.T.);
#3503=ORIENTED_EDGE('',*,*,#2569,.T.);
#3504=ORIENTED_EDGE('',*,*,#2560,.T.);
#3505=ORIENTED_EDGE('',*,*,#2568,.F.);
#3506=ORIENTED_EDGE('',*,*,#2570,.F.);
#3507=ORIENTED_EDGE('',*,*,#2571,.T.);
#3508=ORIENTED_EDGE('',*,*,#2572,.T.);
#3509=ORIENTED_EDGE('',*,*,#2571,.F.);
#3510=ORIENTED_EDGE('',*,*,#2550,.T.);
#3511=ORIENTED_EDGE('',*,*,#2573,.T.);
#3512=ORIENTED_EDGE('',*,*,#2561,.T.);
#3513=ORIENTED_EDGE('',*,*,#2569,.F.);
#3514=ORIENTED_EDGE('',*,*,#2556,.T.);
#3515=ORIENTED_EDGE('',*,*,#2567,.T.);
#3516=ORIENTED_EDGE('',*,*,#2563,.T.);
#3517=ORIENTED_EDGE('',*,*,#2574,.F.);
#3518=ORIENTED_EDGE('',*,*,#2557,.T.);
#3519=ORIENTED_EDGE('',*,*,#2574,.T.);
#3520=ORIENTED_EDGE('',*,*,#2562,.T.);
#3521=ORIENTED_EDGE('',*,*,#2573,.F.);
#3522=ORIENTED_EDGE('',*,*,#2558,.T.);
#3523=ORIENTED_EDGE('',*,*,#2570,.T.);
#3524=ORIENTED_EDGE('',*,*,#2553,.T.);
#3525=ORIENTED_EDGE('',*,*,#2572,.F.);
#3526=ORIENTED_EDGE('',*,*,#2575,.F.);
#3527=ORIENTED_EDGE('',*,*,#2576,.T.);
#3528=ORIENTED_EDGE('',*,*,#2577,.F.);
#3529=ORIENTED_EDGE('',*,*,#2576,.F.);
#3530=ORIENTED_EDGE('',*,*,#2578,.T.);
#3531=ORIENTED_EDGE('',*,*,#2579,.T.);
#3532=ORIENTED_EDGE('',*,*,#2580,.F.);
#3533=ORIENTED_EDGE('',*,*,#2581,.F.);
#3534=ORIENTED_EDGE('',*,*,#2577,.T.);
#3535=ORIENTED_EDGE('',*,*,#2582,.T.);
#3536=ORIENTED_EDGE('',*,*,#2581,.T.);
#3537=ORIENTED_EDGE('',*,*,#2583,.F.);
#3538=ORIENTED_EDGE('',*,*,#2584,.F.);
#3539=ORIENTED_EDGE('',*,*,#2585,.T.);
#3540=ORIENTED_EDGE('',*,*,#2584,.T.);
#3541=ORIENTED_EDGE('',*,*,#2586,.F.);
#3542=ORIENTED_EDGE('',*,*,#2587,.F.);
#3543=ORIENTED_EDGE('',*,*,#2575,.T.);
#3544=ORIENTED_EDGE('',*,*,#2588,.T.);
#3545=ORIENTED_EDGE('',*,*,#2587,.T.);
#3546=ORIENTED_EDGE('',*,*,#2589,.F.);
#3547=ORIENTED_EDGE('',*,*,#2579,.F.);
#3548=ORIENTED_EDGE('',*,*,#2589,.T.);
#3549=ORIENTED_EDGE('',*,*,#2586,.T.);
#3550=ORIENTED_EDGE('',*,*,#2583,.T.);
#3551=ORIENTED_EDGE('',*,*,#2580,.T.);
#3552=ORIENTED_EDGE('',*,*,#2588,.F.);
#3553=ORIENTED_EDGE('',*,*,#2578,.F.);
#3554=ORIENTED_EDGE('',*,*,#2582,.F.);
#3555=ORIENTED_EDGE('',*,*,#2585,.F.);
#3556=CYLINDRICAL_SURFACE('',#3997,0.274999999999999);
#3557=CYLINDRICAL_SURFACE('',#4000,0.274999999999999);
#3558=CYLINDRICAL_SURFACE('',#4046,0.21);
#3559=CYLINDRICAL_SURFACE('',#4060,0.275);
#3560=CYLINDRICAL_SURFACE('',#4063,0.275);
#3561=CYLINDRICAL_SURFACE('',#4066,0.31);
#3562=CYLINDRICAL_SURFACE('',#4069,0.31);
#3563=CYLINDRICAL_SURFACE('',#4075,0.6);
#3564=CYLINDRICAL_SURFACE('',#4082,0.6);
#3565=CYLINDRICAL_SURFACE('',#4089,0.08);
#3566=CYLINDRICAL_SURFACE('',#4094,0.5);
#3567=CYLINDRICAL_SURFACE('',#4098,0.3);
#3568=CYLINDRICAL_SURFACE('',#4104,0.32);
#3569=CYLINDRICAL_SURFACE('',#4107,0.6);
#3570=CYLINDRICAL_SURFACE('',#4119,0.08);
#3571=CYLINDRICAL_SURFACE('',#4126,0.2117);
#3572=CYLINDRICAL_SURFACE('',#4155,0.425);
#3573=CYLINDRICAL_SURFACE('',#4163,0.24505);
#3574=CYLINDRICAL_SURFACE('',#4166,0.274999999999999);
#3575=CYLINDRICAL_SURFACE('',#4169,0.225);
#3576=CYLINDRICAL_SURFACE('',#4172,0.225);
#3577=CYLINDRICAL_SURFACE('',#4175,0.225);
#3578=CYLINDRICAL_SURFACE('',#4178,0.225);
#3579=CYLINDRICAL_SURFACE('',#4188,0.225);
#3580=CYLINDRICAL_SURFACE('',#4191,0.225);
#3581=CYLINDRICAL_SURFACE('',#4194,0.31);
#3582=CYLINDRICAL_SURFACE('',#4206,0.6);
#3583=CYLINDRICAL_SURFACE('',#4214,0.35);
#3584=CYLINDRICAL_SURFACE('',#4222,0.1954);
#3585=CYLINDRICAL_SURFACE('',#4243,0.1666);
#3586=CYLINDRICAL_SURFACE('',#4255,0.265);
#3587=CYLINDRICAL_SURFACE('',#4259,0.5);
#3588=CYLINDRICAL_SURFACE('',#4298,0.425);
#3589=CYLINDRICAL_SURFACE('',#4306,0.24505);
#3590=CYLINDRICAL_SURFACE('',#4327,0.2117);
#3591=CYLINDRICAL_SURFACE('',#4351,0.274999999999999);
#3592=ADVANCED_FACE('',(#523),#3556,.F.);
#3593=ADVANCED_FACE('',(#524),#3557,.F.);
#3594=ADVANCED_FACE('',(#525,#325,#326),#372,.T.);
#3595=ADVANCED_FACE('',(#526),#373,.T.);
#3596=ADVANCED_FACE('',(#527,#327,#328),#374,.T.);
#3597=ADVANCED_FACE('',(#528),#375,.T.);
#3598=ADVANCED_FACE('',(#529),#376,.T.);
#3599=ADVANCED_FACE('',(#530),#377,.F.);
#3600=ADVANCED_FACE('',(#531),#378,.F.);
#3601=ADVANCED_FACE('',(#532),#379,.F.);
#3602=ADVANCED_FACE('',(#533),#380,.F.);
#3603=ADVANCED_FACE('',(#534),#381,.F.);
#3604=ADVANCED_FACE('',(#535),#382,.F.);
#3605=ADVANCED_FACE('',(#536),#383,.F.);
#3606=ADVANCED_FACE('',(#537),#384,.F.);
#3607=ADVANCED_FACE('',(#538),#385,.F.);
#3608=ADVANCED_FACE('',(#539),#386,.F.);
#3609=ADVANCED_FACE('',(#540),#387,.F.);
#3610=ADVANCED_FACE('',(#541),#388,.F.);
#3611=ADVANCED_FACE('',(#542),#389,.F.);
#3612=ADVANCED_FACE('',(#543),#390,.F.);
#3613=ADVANCED_FACE('',(#544),#391,.F.);
#3614=ADVANCED_FACE('',(#545),#392,.F.);
#3615=ADVANCED_FACE('',(#546),#393,.F.);
#3616=ADVANCED_FACE('',(#547),#394,.F.);
#3617=ADVANCED_FACE('',(#548),#395,.F.);
#3618=ADVANCED_FACE('',(#549),#396,.F.);
#3619=ADVANCED_FACE('',(#550),#397,.F.);
#3620=ADVANCED_FACE('',(#551),#398,.F.);
#3621=ADVANCED_FACE('',(#552),#399,.F.);
#3622=ADVANCED_FACE('',(#553),#400,.F.);
#3623=ADVANCED_FACE('',(#554),#401,.F.);
#3624=ADVANCED_FACE('',(#555),#402,.F.);
#3625=ADVANCED_FACE('',(#556),#403,.F.);
#3626=ADVANCED_FACE('',(#557),#404,.F.);
#3627=ADVANCED_FACE('',(#558),#405,.F.);
#3628=ADVANCED_FACE('',(#559),#406,.F.);
#3629=ADVANCED_FACE('',(#560),#407,.F.);
#3630=ADVANCED_FACE('',(#561),#408,.F.);
#3631=ADVANCED_FACE('',(#562),#409,.F.);
#3632=ADVANCED_FACE('',(#563),#410,.F.);
#3633=ADVANCED_FACE('',(#564),#411,.F.);
#3634=ADVANCED_FACE('',(#565),#412,.F.);
#3635=ADVANCED_FACE('',(#566),#413,.F.);
#3636=ADVANCED_FACE('',(#567),#3558,.F.);
#3637=ADVANCED_FACE('',(#568),#414,.T.);
#3638=ADVANCED_FACE('',(#569),#415,.T.);
#3639=ADVANCED_FACE('',(#570),#416,.T.);
#3640=ADVANCED_FACE('',(#571),#417,.T.);
#3641=ADVANCED_FACE('',(#572),#418,.T.);
#3642=ADVANCED_FACE('',(#573),#419,.T.);
#3643=ADVANCED_FACE('',(#574),#420,.T.);
#3644=ADVANCED_FACE('',(#575),#421,.T.);
#3645=ADVANCED_FACE('',(#576,#329),#422,.T.);
#3646=ADVANCED_FACE('',(#577,#330),#423,.F.);
#3647=ADVANCED_FACE('',(#578),#3559,.F.);
#3648=ADVANCED_FACE('',(#579),#3560,.F.);
#3649=ADVANCED_FACE('',(#580),#3561,.F.);
#3650=ADVANCED_FACE('',(#581),#3562,.F.);
#3651=ADVANCED_FACE('',(#582),#424,.F.);
#3652=ADVANCED_FACE('',(#583),#425,.F.);
#3653=ADVANCED_FACE('',(#584,#331,#332),#426,.T.);
#3654=ADVANCED_FACE('',(#585),#3563,.T.);
#3655=ADVANCED_FACE('',(#586,#333),#427,.F.);
#3656=ADVANCED_FACE('',(#587),#428,.T.);
#3657=ADVANCED_FACE('',(#588,#334),#429,.T.);
#3658=ADVANCED_FACE('',(#589),#3564,.T.);
#3659=ADVANCED_FACE('',(#590,#335),#430,.F.);
#3660=ADVANCED_FACE('',(#591,#336,#337),#431,.T.);
#3661=ADVANCED_FACE('',(#592),#432,.T.);
#3662=ADVANCED_FACE('',(#593,#338),#433,.T.);
#3663=ADVANCED_FACE('',(#594),#3565,.F.);
#3664=ADVANCED_FACE('',(#595),#434,.T.);
#3665=ADVANCED_FACE('',(#596),#240,.T.);
#3666=ADVANCED_FACE('',(#597),#3566,.T.);
#3667=ADVANCED_FACE('',(#598,#339),#435,.T.);
#3668=ADVANCED_FACE('',(#599,#340),#3567,.T.);
#3669=ADVANCED_FACE('',(#600),#241,.T.);
#3670=ADVANCED_FACE('',(#601),#436,.T.);
#3671=ADVANCED_FACE('',(#602),#3568,.F.);
#3672=ADVANCED_FACE('',(#603),#3569,.T.);
#3673=ADVANCED_FACE('',(#604,#341),#437,.T.);
#3674=ADVANCED_FACE('',(#605,#342),#438,.F.);
#3675=ADVANCED_FACE('',(#606,#343),#239,.T.);
#3676=ADVANCED_FACE('',(#607),#439,.F.);
#3677=ADVANCED_FACE('',(#608),#440,.T.);
#3678=ADVANCED_FACE('',(#609),#3570,.T.);
#3679=ADVANCED_FACE('',(#610),#441,.F.);
#3680=ADVANCED_FACE('',(#611),#442,.T.);
#3681=ADVANCED_FACE('',(#612),#3571,.F.);
#3682=ADVANCED_FACE('',(#613),#443,.F.);
#3683=ADVANCED_FACE('',(#614),#444,.F.);
#3684=ADVANCED_FACE('',(#615),#445,.T.);
#3685=ADVANCED_FACE('',(#616),#446,.T.);
#3686=ADVANCED_FACE('',(#617),#447,.T.);
#3687=ADVANCED_FACE('',(#618),#448,.T.);
#3688=ADVANCED_FACE('',(#619),#449,.T.);
#3689=ADVANCED_FACE('',(#620,#344),#450,.T.);
#3690=ADVANCED_FACE('',(#621),#451,.F.);
#3691=ADVANCED_FACE('',(#622),#452,.F.);
#3692=ADVANCED_FACE('',(#623),#453,.F.);
#3693=ADVANCED_FACE('',(#624),#454,.F.);
#3694=ADVANCED_FACE('',(#625),#455,.F.);
#3695=ADVANCED_FACE('',(#626),#456,.F.);
#3696=ADVANCED_FACE('',(#627),#457,.F.);
#3697=ADVANCED_FACE('',(#628),#458,.F.);
#3698=ADVANCED_FACE('',(#629),#459,.F.);
#3699=ADVANCED_FACE('',(#630),#460,.T.);
#3700=ADVANCED_FACE('',(#631),#242,.T.);
#3701=ADVANCED_FACE('',(#632),#3572,.T.);
#3702=ADVANCED_FACE('',(#633),#243,.T.);
#3703=ADVANCED_FACE('',(#634,#345),#461,.T.);
#3704=ADVANCED_FACE('',(#635),#244,.T.);
#3705=ADVANCED_FACE('',(#636),#3573,.T.);
#3706=ADVANCED_FACE('',(#637),#3574,.F.);
#3707=ADVANCED_FACE('',(#638),#3575,.F.);
#3708=ADVANCED_FACE('',(#639),#3576,.F.);
#3709=ADVANCED_FACE('',(#640),#3577,.F.);
#3710=ADVANCED_FACE('',(#641),#3578,.F.);
#3711=ADVANCED_FACE('',(#642,#346,#347,#348,#349,#350),#462,.T.);
#3712=ADVANCED_FACE('',(#643),#463,.T.);
#3713=ADVANCED_FACE('',(#644,#351,#352,#353,#354,#355),#464,.T.);
#3714=ADVANCED_FACE('',(#645),#465,.T.);
#3715=ADVANCED_FACE('',(#646),#466,.T.);
#3716=ADVANCED_FACE('',(#647),#467,.F.);
#3717=ADVANCED_FACE('',(#648),#3579,.F.);
#3718=ADVANCED_FACE('',(#649),#3580,.F.);
#3719=ADVANCED_FACE('',(#650),#3581,.F.);
#3720=ADVANCED_FACE('',(#651),#468,.T.);
#3721=ADVANCED_FACE('',(#652),#469,.T.);
#3722=ADVANCED_FACE('',(#653),#470,.T.);
#3723=ADVANCED_FACE('',(#654),#471,.T.);
#3724=ADVANCED_FACE('',(#655),#472,.T.);
#3725=ADVANCED_FACE('',(#656,#356),#473,.F.);
#3726=ADVANCED_FACE('',(#657,#357,#358),#474,.F.);
#3727=ADVANCED_FACE('',(#658,#359,#360),#475,.T.);
#3728=ADVANCED_FACE('',(#659),#3582,.T.);
#3729=ADVANCED_FACE('',(#660,#361),#476,.T.);
#3730=ADVANCED_FACE('',(#661),#477,.T.);
#3731=ADVANCED_FACE('',(#662),#245,.T.);
#3732=ADVANCED_FACE('',(#663),#3583,.T.);
#3733=ADVANCED_FACE('',(#664),#246,.T.);
#3734=ADVANCED_FACE('',(#665,#362),#478,.T.);
#3735=ADVANCED_FACE('',(#666),#247,.T.);
#3736=ADVANCED_FACE('',(#667),#3584,.T.);
#3737=ADVANCED_FACE('',(#668),#248,.T.);
#3738=ADVANCED_FACE('',(#669),#479,.T.);
#3739=ADVANCED_FACE('',(#670),#480,.F.);
#3740=ADVANCED_FACE('',(#671),#481,.F.);
#3741=ADVANCED_FACE('',(#672),#482,.F.);
#3742=ADVANCED_FACE('',(#673),#483,.F.);
#3743=ADVANCED_FACE('',(#674),#484,.F.);
#3744=ADVANCED_FACE('',(#675),#485,.F.);
#3745=ADVANCED_FACE('',(#676),#486,.F.);
#3746=ADVANCED_FACE('',(#677),#487,.F.);
#3747=ADVANCED_FACE('',(#678),#249,.T.);
#3748=ADVANCED_FACE('',(#679),#250,.T.);
#3749=ADVANCED_FACE('',(#680),#488,.T.);
#3750=ADVANCED_FACE('',(#681),#489,.T.);
#3751=ADVANCED_FACE('',(#682),#490,.T.);
#3752=ADVANCED_FACE('',(#683),#3585,.F.);
#3753=ADVANCED_FACE('',(#684),#491,.T.);
#3754=ADVANCED_FACE('',(#685),#492,.T.);
#3755=ADVANCED_FACE('',(#686),#493,.T.);
#3756=ADVANCED_FACE('',(#687,#363),#494,.T.);
#3757=ADVANCED_FACE('',(#688,#364),#495,.F.);
#3758=ADVANCED_FACE('',(#689),#251,.F.);
#3759=ADVANCED_FACE('',(#690),#3586,.F.);
#3760=ADVANCED_FACE('',(#691,#365),#496,.T.);
#3761=ADVANCED_FACE('',(#692),#3587,.T.);
#3762=ADVANCED_FACE('',(#693,#366),#497,.F.);
#3763=ADVANCED_FACE('',(#694),#498,.T.);
#3764=ADVANCED_FACE('',(#695),#252,.T.);
#3765=ADVANCED_FACE('',(#696),#3588,.T.);
#3766=ADVANCED_FACE('',(#697),#253,.T.);
#3767=ADVANCED_FACE('',(#698,#367),#499,.T.);
#3768=ADVANCED_FACE('',(#699),#254,.T.);
#3769=ADVANCED_FACE('',(#700),#3589,.T.);
#3770=ADVANCED_FACE('',(#701),#255,.T.);
#3771=ADVANCED_FACE('',(#702),#500,.T.);
#3772=ADVANCED_FACE('',(#703),#501,.F.);
#3773=ADVANCED_FACE('',(#704),#502,.F.);
#3774=ADVANCED_FACE('',(#705),#503,.F.);
#3775=ADVANCED_FACE('',(#706),#504,.F.);
#3776=ADVANCED_FACE('',(#707),#505,.F.);
#3777=ADVANCED_FACE('',(#708),#506,.F.);
#3778=ADVANCED_FACE('',(#709),#507,.F.);
#3779=ADVANCED_FACE('',(#710),#508,.F.);
#3780=ADVANCED_FACE('',(#711),#256,.T.);
#3781=ADVANCED_FACE('',(#712),#257,.T.);
#3782=ADVANCED_FACE('',(#713),#509,.T.);
#3783=ADVANCED_FACE('',(#714),#510,.T.);
#3784=ADVANCED_FACE('',(#715),#511,.T.);
#3785=ADVANCED_FACE('',(#716),#3590,.F.);
#3786=ADVANCED_FACE('',(#717),#512,.T.);
#3787=ADVANCED_FACE('',(#718),#513,.T.);
#3788=ADVANCED_FACE('',(#719),#514,.T.);
#3789=ADVANCED_FACE('',(#720,#368),#515,.T.);
#3790=ADVANCED_FACE('',(#721,#369),#516,.F.);
#3791=ADVANCED_FACE('',(#722),#3591,.F.);
#3792=ADVANCED_FACE('',(#723,#370),#517,.T.);
#3793=ADVANCED_FACE('',(#724),#518,.T.);
#3794=ADVANCED_FACE('',(#725,#371),#519,.T.);
#3795=ADVANCED_FACE('',(#726),#520,.T.);
#3796=ADVANCED_FACE('',(#727),#521,.T.);
#3797=ADVANCED_FACE('',(#728),#522,.F.);
#3798=CLOSED_SHELL('',(#3592,#3593,#3594,#3595,#3596,#3597,#3598,#3599));
#3799=CLOSED_SHELL('',(#3600,#3601,#3602,#3603,#3604,#3605,#3606,#3607,
#3608,#3609,#3610,#3611,#3612,#3613,#3614,#3615,#3616,#3617,#3618,#3619,
#3620,#3621,#3622,#3623,#3624,#3625,#3626,#3627,#3628,#3629,#3630,#3631,
#3632,#3633,#3634,#3635,#3636,#3637,#3638,#3639,#3640,#3641,#3642,#3643,
#3644,#3645,#3646));
#3800=CLOSED_SHELL('',(#3647,#3648,#3649,#3650,#3651,#3652,#3653,#3654,
#3655,#3656,#3657,#3658,#3659,#3660,#3661,#3662));
#3801=CLOSED_SHELL('',(#3663,#3664,#3665,#3666,#3667,#3668,#3669,#3670));
#3802=CLOSED_SHELL('',(#3671,#3672,#3673,#3674));
#3803=CLOSED_SHELL('',(#3675,#3676,#3677,#3678,#3679));
#3804=CLOSED_SHELL('',(#3680,#3681,#3682,#3683,#3684,#3685,#3686,#3687,
#3688,#3689));
#3805=CLOSED_SHELL('',(#3690,#3691,#3692,#3693,#3694,#3695,#3696,#3697));
#3806=CLOSED_SHELL('',(#3698,#3699,#3700,#3701,#3702,#3703,#3704,#3705));
#3807=CLOSED_SHELL('',(#3706,#3707,#3708,#3709,#3710,#3711,#3712,#3713,
#3714,#3715,#3716));
#3808=CLOSED_SHELL('',(#3717,#3718,#3719,#3720,#3721,#3722,#3723,#3724,
#3725,#3726,#3727,#3728,#3729));
#3809=CLOSED_SHELL('',(#3730,#3731,#3732,#3733,#3734,#3735,#3736,#3737,
#3738));
#3810=CLOSED_SHELL('',(#3739,#3740,#3741,#3742,#3743,#3744,#3745,#3746));
#3811=CLOSED_SHELL('',(#3747,#3748,#3749,#3750,#3751,#3752,#3753,#3754,
#3755,#3756,#3757));
#3812=CLOSED_SHELL('',(#3758,#3759,#3760,#3761,#3762));
#3813=CLOSED_SHELL('',(#3763,#3764,#3765,#3766,#3767,#3768,#3769,#3770,
#3771));
#3814=CLOSED_SHELL('',(#3772,#3773,#3774,#3775,#3776,#3777,#3778,#3779));
#3815=CLOSED_SHELL('',(#3780,#3781,#3782,#3783,#3784,#3785,#3786,#3787,
#3788,#3789,#3790));
#3816=CLOSED_SHELL('',(#3791,#3792,#3793,#3794,#3795,#3796,#3797));
#3817=DERIVED_UNIT_ELEMENT(#3849,1.);
#3818=DERIVED_UNIT_ELEMENT(#6745,-3.);
#3819=DERIVED_UNIT_ELEMENT(#3849,1.);
#3820=DERIVED_UNIT_ELEMENT(#6745,-3.);
#3821=DERIVED_UNIT_ELEMENT(#3849,1.);
#3822=DERIVED_UNIT_ELEMENT(#6745,-3.);
#3823=DERIVED_UNIT_ELEMENT(#3849,1.);
#3824=DERIVED_UNIT_ELEMENT(#6745,-3.);
#3825=DERIVED_UNIT_ELEMENT(#3849,1.);
#3826=DERIVED_UNIT_ELEMENT(#6745,-3.);
#3827=DERIVED_UNIT_ELEMENT(#3849,1.);
#3828=DERIVED_UNIT_ELEMENT(#6745,-3.);
#3829=DERIVED_UNIT_ELEMENT(#3849,1.);
#3830=DERIVED_UNIT_ELEMENT(#6745,-3.);
#3831=DERIVED_UNIT_ELEMENT(#3849,1.);
#3832=DERIVED_UNIT_ELEMENT(#6745,-3.);
#3833=DERIVED_UNIT_ELEMENT(#3849,1.);
#3834=DERIVED_UNIT_ELEMENT(#6745,-3.);
#3835=DERIVED_UNIT_ELEMENT(#3849,1.);
#3836=DERIVED_UNIT_ELEMENT(#6745,-3.);
#3837=DERIVED_UNIT_ELEMENT(#3849,1.);
#3838=DERIVED_UNIT_ELEMENT(#6745,-3.);
#3839=DERIVED_UNIT_ELEMENT(#3849,1.);
#3840=DERIVED_UNIT_ELEMENT(#6745,-3.);
#3841=DERIVED_UNIT_ELEMENT(#3849,1.);
#3842=DERIVED_UNIT_ELEMENT(#6745,-3.);
#3843=DERIVED_UNIT_ELEMENT(#3849,1.);
#3844=DERIVED_UNIT_ELEMENT(#6745,-3.);
#3845=DERIVED_UNIT_ELEMENT(#3849,1.);
#3846=DERIVED_UNIT_ELEMENT(#6745,-3.);
#3847=DERIVED_UNIT_ELEMENT(#3849,1.);
#3848=DERIVED_UNIT_ELEMENT(#6745,-3.);
#3849=(
MASS_UNIT()
NAMED_UNIT(*)
SI_UNIT(.KILO.,.GRAM.)
);
#3850=DERIVED_UNIT((#3817,#3818));
#3851=DERIVED_UNIT((#3819,#3820));
#3852=DERIVED_UNIT((#3821,#3822));
#3853=DERIVED_UNIT((#3823,#3824));
#3854=DERIVED_UNIT((#3825,#3826));
#3855=DERIVED_UNIT((#3827,#3828));
#3856=DERIVED_UNIT((#3829,#3830));
#3857=DERIVED_UNIT((#3831,#3832));
#3858=DERIVED_UNIT((#3833,#3834));
#3859=DERIVED_UNIT((#3835,#3836));
#3860=DERIVED_UNIT((#3837,#3838));
#3861=DERIVED_UNIT((#3839,#3840));
#3862=DERIVED_UNIT((#3841,#3842));
#3863=DERIVED_UNIT((#3843,#3844));
#3864=DERIVED_UNIT((#3845,#3846));
#3865=DERIVED_UNIT((#3847,#3848));
#3866=MEASURE_REPRESENTATION_ITEM('density measure',
POSITIVE_RATIO_MEASURE(7850.),#3850);
#3867=MEASURE_REPRESENTATION_ITEM('density measure',
POSITIVE_RATIO_MEASURE(7850.),#3851);
#3868=MEASURE_REPRESENTATION_ITEM('density measure',
POSITIVE_RATIO_MEASURE(7850.),#3852);
#3869=MEASURE_REPRESENTATION_ITEM('density measure',
POSITIVE_RATIO_MEASURE(7850.),#3853);
#3870=MEASURE_REPRESENTATION_ITEM('density measure',
POSITIVE_RATIO_MEASURE(7850.),#3854);
#3871=MEASURE_REPRESENTATION_ITEM('density measure',
POSITIVE_RATIO_MEASURE(7850.),#3855);
#3872=MEASURE_REPRESENTATION_ITEM('density measure',
POSITIVE_RATIO_MEASURE(7850.),#3856);
#3873=MEASURE_REPRESENTATION_ITEM('density measure',
POSITIVE_RATIO_MEASURE(7850.),#3857);
#3874=MEASURE_REPRESENTATION_ITEM('density measure',
POSITIVE_RATIO_MEASURE(7850.),#3858);
#3875=MEASURE_REPRESENTATION_ITEM('density measure',
POSITIVE_RATIO_MEASURE(7850.),#3859);
#3876=MEASURE_REPRESENTATION_ITEM('density measure',
POSITIVE_RATIO_MEASURE(7850.),#3860);
#3877=MEASURE_REPRESENTATION_ITEM('density measure',
POSITIVE_RATIO_MEASURE(7850.),#3861);
#3878=MEASURE_REPRESENTATION_ITEM('density measure',
POSITIVE_RATIO_MEASURE(7850.),#3862);
#3879=MEASURE_REPRESENTATION_ITEM('density measure',
POSITIVE_RATIO_MEASURE(7850.),#3863);
#3880=MEASURE_REPRESENTATION_ITEM('density measure',
POSITIVE_RATIO_MEASURE(7850.),#3864);
#3881=MEASURE_REPRESENTATION_ITEM('density measure',
POSITIVE_RATIO_MEASURE(7850.),#3865);
#3882=PROPERTY_DEFINITION_REPRESENTATION(#3962,#3914);
#3883=PROPERTY_DEFINITION_REPRESENTATION(#3963,#3915);
#3884=PROPERTY_DEFINITION_REPRESENTATION(#3964,#3916);
#3885=PROPERTY_DEFINITION_REPRESENTATION(#3965,#3917);
#3886=PROPERTY_DEFINITION_REPRESENTATION(#3966,#3918);
#3887=PROPERTY_DEFINITION_REPRESENTATION(#3967,#3919);
#3888=PROPERTY_DEFINITION_REPRESENTATION(#3968,#3920);
#3889=PROPERTY_DEFINITION_REPRESENTATION(#3969,#3921);
#3890=PROPERTY_DEFINITION_REPRESENTATION(#3970,#3922);
#3891=PROPERTY_DEFINITION_REPRESENTATION(#3971,#3923);
#3892=PROPERTY_DEFINITION_REPRESENTATION(#3972,#3924);
#3893=PROPERTY_DEFINITION_REPRESENTATION(#3973,#3925);
#3894=PROPERTY_DEFINITION_REPRESENTATION(#3974,#3926);
#3895=PROPERTY_DEFINITION_REPRESENTATION(#3975,#3927);
#3896=PROPERTY_DEFINITION_REPRESENTATION(#3976,#3928);
#3897=PROPERTY_DEFINITION_REPRESENTATION(#3977,#3929);
#3898=PROPERTY_DEFINITION_REPRESENTATION(#3978,#3930);
#3899=PROPERTY_DEFINITION_REPRESENTATION(#3979,#3931);
#3900=PROPERTY_DEFINITION_REPRESENTATION(#3980,#3932);
#3901=PROPERTY_DEFINITION_REPRESENTATION(#3981,#3933);
#3902=PROPERTY_DEFINITION_REPRESENTATION(#3982,#3934);
#3903=PROPERTY_DEFINITION_REPRESENTATION(#3983,#3935);
#3904=PROPERTY_DEFINITION_REPRESENTATION(#3984,#3936);
#3905=PROPERTY_DEFINITION_REPRESENTATION(#3985,#3937);
#3906=PROPERTY_DEFINITION_REPRESENTATION(#3986,#3938);
#3907=PROPERTY_DEFINITION_REPRESENTATION(#3987,#3939);
#3908=PROPERTY_DEFINITION_REPRESENTATION(#3988,#3940);
#3909=PROPERTY_DEFINITION_REPRESENTATION(#3989,#3941);
#3910=PROPERTY_DEFINITION_REPRESENTATION(#3990,#3942);
#3911=PROPERTY_DEFINITION_REPRESENTATION(#3991,#3943);
#3912=PROPERTY_DEFINITION_REPRESENTATION(#3992,#3944);
#3913=PROPERTY_DEFINITION_REPRESENTATION(#3993,#3945);
#3914=REPRESENTATION('material name',(#3946),#6725);
#3915=REPRESENTATION('density',(#3866),#6725);
#3916=REPRESENTATION('material name',(#3947),#6726);
#3917=REPRESENTATION('density',(#3867),#6726);
#3918=REPRESENTATION('material name',(#3948),#6727);
#3919=REPRESENTATION('density',(#3868),#6727);
#3920=REPRESENTATION('material name',(#3949),#6728);
#3921=REPRESENTATION('density',(#3869),#6728);
#3922=REPRESENTATION('material name',(#3950),#6729);
#3923=REPRESENTATION('density',(#3870),#6729);
#3924=REPRESENTATION('material name',(#3951),#6730);
#3925=REPRESENTATION('density',(#3871),#6730);
#3926=REPRESENTATION('material name',(#3952),#6731);
#3927=REPRESENTATION('density',(#3872),#6731);
#3928=REPRESENTATION('material name',(#3953),#6732);
#3929=REPRESENTATION('density',(#3873),#6732);
#3930=REPRESENTATION('material name',(#3954),#6734);
#3931=REPRESENTATION('density',(#3874),#6734);
#3932=REPRESENTATION('material name',(#3955),#6735);
#3933=REPRESENTATION('density',(#3875),#6735);
#3934=REPRESENTATION('material name',(#3956),#6736);
#3935=REPRESENTATION('density',(#3876),#6736);
#3936=REPRESENTATION('material name',(#3957),#6737);
#3937=REPRESENTATION('density',(#3877),#6737);
#3938=REPRESENTATION('material name',(#3958),#6738);
#3939=REPRESENTATION('density',(#3878),#6738);
#3940=REPRESENTATION('material name',(#3959),#6739);
#3941=REPRESENTATION('density',(#3879),#6739);
#3942=REPRESENTATION('material name',(#3960),#6740);
#3943=REPRESENTATION('density',(#3880),#6740);
#3944=REPRESENTATION('material name',(#3961),#6742);
#3945=REPRESENTATION('density',(#3881),#6742);
#3946=DESCRIPTIVE_REPRESENTATION_ITEM('Steel','Steel');
#3947=DESCRIPTIVE_REPRESENTATION_ITEM('Steel','Steel');
#3948=DESCRIPTIVE_REPRESENTATION_ITEM('Steel','Steel');
#3949=DESCRIPTIVE_REPRESENTATION_ITEM('Steel','Steel');
#3950=DESCRIPTIVE_REPRESENTATION_ITEM('Steel','Steel');
#3951=DESCRIPTIVE_REPRESENTATION_ITEM('Steel','Steel');
#3952=DESCRIPTIVE_REPRESENTATION_ITEM('Steel','Steel');
#3953=DESCRIPTIVE_REPRESENTATION_ITEM('Steel','Steel');
#3954=DESCRIPTIVE_REPRESENTATION_ITEM('Steel','Steel');
#3955=DESCRIPTIVE_REPRESENTATION_ITEM('Steel','Steel');
#3956=DESCRIPTIVE_REPRESENTATION_ITEM('Steel','Steel');
#3957=DESCRIPTIVE_REPRESENTATION_ITEM('Steel','Steel');
#3958=DESCRIPTIVE_REPRESENTATION_ITEM('Steel','Steel');
#3959=DESCRIPTIVE_REPRESENTATION_ITEM('Steel','Steel');
#3960=DESCRIPTIVE_REPRESENTATION_ITEM('Steel','Steel');
#3961=DESCRIPTIVE_REPRESENTATION_ITEM('Steel','Steel');
#3962=PROPERTY_DEFINITION('material property','material name',#6860);
#3963=PROPERTY_DEFINITION('material property','density of part',#6860);
#3964=PROPERTY_DEFINITION('material property','material name',#6861);
#3965=PROPERTY_DEFINITION('material property','density of part',#6861);
#3966=PROPERTY_DEFINITION('material property','material name',#6862);
#3967=PROPERTY_DEFINITION('material property','density of part',#6862);
#3968=PROPERTY_DEFINITION('material property','material name',#6863);
#3969=PROPERTY_DEFINITION('material property','density of part',#6863);
#3970=PROPERTY_DEFINITION('material property','material name',#6864);
#3971=PROPERTY_DEFINITION('material property','density of part',#6864);
#3972=PROPERTY_DEFINITION('material property','material name',#6865);
#3973=PROPERTY_DEFINITION('material property','density of part',#6865);
#3974=PROPERTY_DEFINITION('material property','material name',#6866);
#3975=PROPERTY_DEFINITION('material property','density of part',#6866);
#3976=PROPERTY_DEFINITION('material property','material name',#6867);
#3977=PROPERTY_DEFINITION('material property','density of part',#6867);
#3978=PROPERTY_DEFINITION('material property','material name',#6869);
#3979=PROPERTY_DEFINITION('material property','density of part',#6869);
#3980=PROPERTY_DEFINITION('material property','material name',#6870);
#3981=PROPERTY_DEFINITION('material property','density of part',#6870);
#3982=PROPERTY_DEFINITION('material property','material name',#6871);
#3983=PROPERTY_DEFINITION('material property','density of part',#6871);
#3984=PROPERTY_DEFINITION('material property','material name',#6872);
#3985=PROPERTY_DEFINITION('material property','density of part',#6872);
#3986=PROPERTY_DEFINITION('material property','material name',#6873);
#3987=PROPERTY_DEFINITION('material property','density of part',#6873);
#3988=PROPERTY_DEFINITION('material property','material name',#6874);
#3989=PROPERTY_DEFINITION('material property','density of part',#6874);
#3990=PROPERTY_DEFINITION('material property','material name',#6875);
#3991=PROPERTY_DEFINITION('material property','density of part',#6875);
#3992=PROPERTY_DEFINITION('material property','material name',#6877);
#3993=PROPERTY_DEFINITION('material property','density of part',#6877);
#3994=AXIS2_PLACEMENT_3D('',#5462,#4364,#4365);
#3995=AXIS2_PLACEMENT_3D('',#5463,#4366,#4367);
#3996=AXIS2_PLACEMENT_3D('',#5464,#4368,#4369);
#3997=AXIS2_PLACEMENT_3D('',#5465,#4370,#4371);
#3998=AXIS2_PLACEMENT_3D('',#5467,#4372,#4373);
#3999=AXIS2_PLACEMENT_3D('',#5470,#4375,#4376);
#4000=AXIS2_PLACEMENT_3D('',#5471,#4377,#4378);
#4001=AXIS2_PLACEMENT_3D('',#5473,#4379,#4380);
#4002=AXIS2_PLACEMENT_3D('',#5476,#4382,#4383);
#4003=AXIS2_PLACEMENT_3D('',#5477,#4384,#4385);
#4004=AXIS2_PLACEMENT_3D('',#5486,#4390,#4391);
#4005=AXIS2_PLACEMENT_3D('',#5492,#4395,#4396);
#4006=AXIS2_PLACEMENT_3D('',#5498,#4400,#4401);
#4007=AXIS2_PLACEMENT_3D('',#5501,#4404,#4405);
#4008=AXIS2_PLACEMENT_3D('',#5502,#4406,#4407);
#4009=AXIS2_PLACEMENT_3D('',#5503,#4408,#4409);
#4010=AXIS2_PLACEMENT_3D('',#5504,#4410,#4411);
#4011=AXIS2_PLACEMENT_3D('',#5513,#4416,#4417);
#4012=AXIS2_PLACEMENT_3D('',#5519,#4421,#4422);
#4013=AXIS2_PLACEMENT_3D('',#5525,#4426,#4427);
#4014=AXIS2_PLACEMENT_3D('',#5531,#4431,#4432);
#4015=AXIS2_PLACEMENT_3D('',#5537,#4436,#4437);
#4016=AXIS2_PLACEMENT_3D('',#5543,#4441,#4442);
#4017=AXIS2_PLACEMENT_3D('',#5549,#4446,#4447);
#4018=AXIS2_PLACEMENT_3D('',#5555,#4451,#4452);
#4019=AXIS2_PLACEMENT_3D('',#5561,#4456,#4457);
#4020=AXIS2_PLACEMENT_3D('',#5570,#4462,#4463);
#4021=AXIS2_PLACEMENT_3D('',#5576,#4467,#4468);
#4022=AXIS2_PLACEMENT_3D('',#5582,#4472,#4473);
#4023=AXIS2_PLACEMENT_3D('',#5588,#4477,#4478);
#4024=AXIS2_PLACEMENT_3D('',#5594,#4482,#4483);
#4025=AXIS2_PLACEMENT_3D('',#5600,#4487,#4488);
#4026=AXIS2_PLACEMENT_3D('',#5606,#4492,#4493);
#4027=AXIS2_PLACEMENT_3D('',#5612,#4497,#4498);
#4028=AXIS2_PLACEMENT_3D('',#5618,#4502,#4503);
#4029=AXIS2_PLACEMENT_3D('',#5627,#4508,#4509);
#4030=AXIS2_PLACEMENT_3D('',#5633,#4513,#4514);
#4031=AXIS2_PLACEMENT_3D('',#5639,#4518,#4519);
#4032=AXIS2_PLACEMENT_3D('',#5645,#4523,#4524);
#4033=AXIS2_PLACEMENT_3D('',#5651,#4528,#4529);
#4034=AXIS2_PLACEMENT_3D('',#5657,#4533,#4534);
#4035=AXIS2_PLACEMENT_3D('',#5663,#4538,#4539);
#4036=AXIS2_PLACEMENT_3D('',#5669,#4543,#4544);
#4037=AXIS2_PLACEMENT_3D('',#5675,#4548,#4549);
#4038=AXIS2_PLACEMENT_3D('',#5684,#4554,#4555);
#4039=AXIS2_PLACEMENT_3D('',#5690,#4559,#4560);
#4040=AXIS2_PLACEMENT_3D('',#5696,#4564,#4565);
#4041=AXIS2_PLACEMENT_3D('',#5702,#4569,#4570);
#4042=AXIS2_PLACEMENT_3D('',#5708,#4574,#4575);
#4043=AXIS2_PLACEMENT_3D('',#5714,#4579,#4580);
#4044=AXIS2_PLACEMENT_3D('',#5720,#4584,#4585);
#4045=AXIS2_PLACEMENT_3D('',#5726,#4589,#4590);
#4046=AXIS2_PLACEMENT_3D('',#5732,#4594,#4595);
#4047=AXIS2_PLACEMENT_3D('',#5734,#4596,#4597);
#4048=AXIS2_PLACEMENT_3D('',#5737,#4599,#4600);
#4049=AXIS2_PLACEMENT_3D('',#5738,#4601,#4602);
#4050=AXIS2_PLACEMENT_3D('',#5744,#4606,#4607);
#4051=AXIS2_PLACEMENT_3D('',#5750,#4611,#4612);
#4052=AXIS2_PLACEMENT_3D('',#5753,#4615,#4616);
#4053=AXIS2_PLACEMENT_3D('',#5759,#4620,#4621);
#4054=AXIS2_PLACEMENT_3D('',#5762,#4624,#4625);
#4055=AXIS2_PLACEMENT_3D('',#5768,#4629,#4630);
#4056=AXIS2_PLACEMENT_3D('',#5771,#4633,#4634);
#4057=AXIS2_PLACEMENT_3D('',#5774,#4637,#4638);
#4058=AXIS2_PLACEMENT_3D('',#5775,#4639,#4640);
#4059=AXIS2_PLACEMENT_3D('',#5776,#4641,#4642);
#4060=AXIS2_PLACEMENT_3D('',#5777,#4643,#4644);
#4061=AXIS2_PLACEMENT_3D('',#5779,#4645,#4646);
#4062=AXIS2_PLACEMENT_3D('',#5782,#4648,#4649);
#4063=AXIS2_PLACEMENT_3D('',#5783,#4650,#4651);
#4064=AXIS2_PLACEMENT_3D('',#5785,#4652,#4653);
#4065=AXIS2_PLACEMENT_3D('',#5788,#4655,#4656);
#4066=AXIS2_PLACEMENT_3D('',#5789,#4657,#4658);
#4067=AXIS2_PLACEMENT_3D('',#5791,#4659,#4660);
#4068=AXIS2_PLACEMENT_3D('',#5794,#4662,#4663);
#4069=AXIS2_PLACEMENT_3D('',#5795,#4664,#4665);
#4070=AXIS2_PLACEMENT_3D('',#5797,#4666,#4667);
#4071=AXIS2_PLACEMENT_3D('',#5800,#4669,#4670);
#4072=AXIS2_PLACEMENT_3D('',#5801,#4671,#4672);
#4073=AXIS2_PLACEMENT_3D('',#5810,#4677,#4678);
#4074=AXIS2_PLACEMENT_3D('',#5816,#4682,#4683);
#4075=AXIS2_PLACEMENT_3D('',#5830,#4691,#4692);
#4076=AXIS2_PLACEMENT_3D('',#5834,#4694,#4695);
#4077=AXIS2_PLACEMENT_3D('',#5835,#4696,#4697);
#4078=AXIS2_PLACEMENT_3D('',#5836,#4698,#4699);
#4079=AXIS2_PLACEMENT_3D('',#5838,#4701,#4702);
#4080=AXIS2_PLACEMENT_3D('',#5848,#4708,#4709);
#4081=AXIS2_PLACEMENT_3D('',#5849,#4710,#4711);
#4082=AXIS2_PLACEMENT_3D('',#5850,#4712,#4713);
#4083=AXIS2_PLACEMENT_3D('',#5851,#4714,#4715);
#4084=AXIS2_PLACEMENT_3D('',#5852,#4716,#4717);
#4085=AXIS2_PLACEMENT_3D('',#5856,#4720,#4721);
#4086=AXIS2_PLACEMENT_3D('',#5860,#4724,#4725);
#4087=AXIS2_PLACEMENT_3D('',#5862,#4727,#4728);
#4088=AXIS2_PLACEMENT_3D('',#5863,#4729,#4730);
#4089=AXIS2_PLACEMENT_3D('',#5864,#4731,#4732);
#4090=AXIS2_PLACEMENT_3D('',#5942,#4734,#4735);
#4091=AXIS2_PLACEMENT_3D('',#5944,#4736,#4737);
#4092=AXIS2_PLACEMENT_3D('',#5945,#4738,#4739);
#4093=AXIS2_PLACEMENT_3D('',#5947,#4740,#4741);
#4094=AXIS2_PLACEMENT_3D('',#5949,#4743,#4744);
#4095=AXIS2_PLACEMENT_3D('',#5951,#4745,#4746);
#4096=AXIS2_PLACEMENT_3D('',#5953,#4748,#4749);
#4097=AXIS2_PLACEMENT_3D('',#5955,#4750,#4751);
#4098=AXIS2_PLACEMENT_3D('',#5956,#4752,#4753);
#4099=AXIS2_PLACEMENT_3D('',#5958,#4754,#4755);
#4100=AXIS2_PLACEMENT_3D('',#5961,#4758,#4759);
#4101=AXIS2_PLACEMENT_3D('',#5963,#4760,#4761);
#4102=AXIS2_PLACEMENT_3D('',#5965,#4763,#4764);
#4103=AXIS2_PLACEMENT_3D('',#5966,#4765,#4766);
#4104=AXIS2_PLACEMENT_3D('',#5967,#4767,#4768);
#4105=AXIS2_PLACEMENT_3D('',#5969,#4769,#4770);
#4106=AXIS2_PLACEMENT_3D('',#5972,#4772,#4773);
#4107=AXIS2_PLACEMENT_3D('',#5973,#4774,#4775);
#4108=AXIS2_PLACEMENT_3D('',#5975,#4776,#4777);
#4109=AXIS2_PLACEMENT_3D('',#5978,#4779,#4780);
#4110=AXIS2_PLACEMENT_3D('',#5979,#4781,#4782);
#4111=AXIS2_PLACEMENT_3D('',#5980,#4783,#4784);
#4112=AXIS2_PLACEMENT_3D('',#5981,#4785,#4786);
#4113=AXIS2_PLACEMENT_3D('',#5982,#4787,#4788);
#4114=AXIS2_PLACEMENT_3D('',#5984,#4789,#4790);
#4115=AXIS2_PLACEMENT_3D('',#5985,#4791,#4792);
#4116=AXIS2_PLACEMENT_3D('',#6040,#4793,#4794);
#4117=AXIS2_PLACEMENT_3D('',#6043,#4795,#4796);
#4118=AXIS2_PLACEMENT_3D('',#6045,#4798,#4799);
#4119=AXIS2_PLACEMENT_3D('',#6051,#4803,#4804);
#4120=AXIS2_PLACEMENT_3D('',#6053,#4805,#4806);
#4121=AXIS2_PLACEMENT_3D('',#6055,#4808,#4809);
#4122=AXIS2_PLACEMENT_3D('',#6056,#4810,#4811);
#4123=AXIS2_PLACEMENT_3D('',#6057,#4812,#4813);
#4124=AXIS2_PLACEMENT_3D('',#6058,#4814,#4815);
#4125=AXIS2_PLACEMENT_3D('',#6069,#4820,#4821);
#4126=AXIS2_PLACEMENT_3D('',#6071,#4823,#4824);
#4127=AXIS2_PLACEMENT_3D('',#6073,#4825,#4826);
#4128=AXIS2_PLACEMENT_3D('',#6076,#4828,#4829);
#4129=AXIS2_PLACEMENT_3D('',#6078,#4830,#4831);
#4130=AXIS2_PLACEMENT_3D('',#6080,#4832,#4833);
#4131=AXIS2_PLACEMENT_3D('',#6081,#4834,#4835);
#4132=AXIS2_PLACEMENT_3D('',#6082,#4836,#4837);
#4133=AXIS2_PLACEMENT_3D('',#6086,#4840,#4841);
#4134=AXIS2_PLACEMENT_3D('',#6090,#4844,#4845);
#4135=AXIS2_PLACEMENT_3D('',#6096,#4849,#4850);
#4136=AXIS2_PLACEMENT_3D('',#6102,#4854,#4855);
#4137=AXIS2_PLACEMENT_3D('',#6106,#4858,#4859);
#4138=AXIS2_PLACEMENT_3D('',#6110,#4862,#4863);
#4139=AXIS2_PLACEMENT_3D('',#6112,#4865,#4866);
#4140=AXIS2_PLACEMENT_3D('',#6113,#4867,#4868);
#4141=AXIS2_PLACEMENT_3D('',#6114,#4869,#4870);
#4142=AXIS2_PLACEMENT_3D('',#6123,#4875,#4876);
#4143=AXIS2_PLACEMENT_3D('',#6129,#4880,#4881);
#4144=AXIS2_PLACEMENT_3D('',#6135,#4885,#4886);
#4145=AXIS2_PLACEMENT_3D('',#6141,#4890,#4891);
#4146=AXIS2_PLACEMENT_3D('',#6147,#4895,#4896);
#4147=AXIS2_PLACEMENT_3D('',#6150,#4899,#4900);
#4148=AXIS2_PLACEMENT_3D('',#6151,#4901,#4902);
#4149=AXIS2_PLACEMENT_3D('',#6152,#4903,#4904);
#4150=AXIS2_PLACEMENT_3D('',#6154,#4905,#4906);
#4151=AXIS2_PLACEMENT_3D('',#6155,#4907,#4908);
#4152=AXIS2_PLACEMENT_3D('',#6157,#4909,#4910);
#4153=AXIS2_PLACEMENT_3D('',#6158,#4911,#4912);
#4154=AXIS2_PLACEMENT_3D('',#6160,#4913,#4914);
#4155=AXIS2_PLACEMENT_3D('',#6162,#4916,#4917);
#4156=AXIS2_PLACEMENT_3D('',#6164,#4918,#4919);
#4157=AXIS2_PLACEMENT_3D('',#6166,#4921,#4922);
#4158=AXIS2_PLACEMENT_3D('',#6168,#4923,#4924);
#4159=AXIS2_PLACEMENT_3D('',#6170,#4926,#4927);
#4160=AXIS2_PLACEMENT_3D('',#6172,#4928,#4929);
#4161=AXIS2_PLACEMENT_3D('',#6173,#4930,#4931);
#4162=AXIS2_PLACEMENT_3D('',#6175,#4932,#4933);
#4163=AXIS2_PLACEMENT_3D('',#6177,#4935,#4936);
#4164=AXIS2_PLACEMENT_3D('',#6179,#4938,#4939);
#4165=AXIS2_PLACEMENT_3D('',#6180,#4940,#4941);
#4166=AXIS2_PLACEMENT_3D('',#6181,#4942,#4943);
#4167=AXIS2_PLACEMENT_3D('',#6183,#4944,#4945);
#4168=AXIS2_PLACEMENT_3D('',#6186,#4947,#4948);
#4169=AXIS2_PLACEMENT_3D('',#6187,#4949,#4950);
#4170=AXIS2_PLACEMENT_3D('',#6189,#4951,#4952);
#4171=AXIS2_PLACEMENT_3D('',#6192,#4954,#4955);
#4172=AXIS2_PLACEMENT_3D('',#6193,#4956,#4957);
#4173=AXIS2_PLACEMENT_3D('',#6195,#4958,#4959);
#4174=AXIS2_PLACEMENT_3D('',#6198,#4961,#4962);
#4175=AXIS2_PLACEMENT_3D('',#6199,#4963,#4964);
#4176=AXIS2_PLACEMENT_3D('',#6201,#4965,#4966);
#4177=AXIS2_PLACEMENT_3D('',#6204,#4968,#4969);
#4178=AXIS2_PLACEMENT_3D('',#6205,#4970,#4971);
#4179=AXIS2_PLACEMENT_3D('',#6207,#4972,#4973);
#4180=AXIS2_PLACEMENT_3D('',#6210,#4975,#4976);
#4181=AXIS2_PLACEMENT_3D('',#6211,#4977,#4978);
#4182=AXIS2_PLACEMENT_3D('',#6220,#4983,#4984);
#4183=AXIS2_PLACEMENT_3D('',#6226,#4988,#4989);
#4184=AXIS2_PLACEMENT_3D('',#6232,#4993,#4994);
#4185=AXIS2_PLACEMENT_3D('',#6235,#4997,#4998);
#4186=AXIS2_PLACEMENT_3D('',#6236,#4999,#5000);
#4187=AXIS2_PLACEMENT_3D('',#6237,#5001,#5002);
#4188=AXIS2_PLACEMENT_3D('',#6238,#5003,#5004);
#4189=AXIS2_PLACEMENT_3D('',#6240,#5005,#5006);
#4190=AXIS2_PLACEMENT_3D('',#6243,#5008,#5009);
#4191=AXIS2_PLACEMENT_3D('',#6244,#5010,#5011);
#4192=AXIS2_PLACEMENT_3D('',#6246,#5012,#5013);
#4193=AXIS2_PLACEMENT_3D('',#6249,#5015,#5016);
#4194=AXIS2_PLACEMENT_3D('',#6250,#5017,#5018);
#4195=AXIS2_PLACEMENT_3D('',#6252,#5019,#5020);
#4196=AXIS2_PLACEMENT_3D('',#6255,#5022,#5023);
#4197=AXIS2_PLACEMENT_3D('',#6256,#5024,#5025);
#4198=AXIS2_PLACEMENT_3D('',#6265,#5030,#5031);
#4199=AXIS2_PLACEMENT_3D('',#6274,#5036,#5037);
#4200=AXIS2_PLACEMENT_3D('',#6280,#5041,#5042);
#4201=AXIS2_PLACEMENT_3D('',#6286,#5046,#5047);
#4202=AXIS2_PLACEMENT_3D('',#6289,#5050,#5051);
#4203=AXIS2_PLACEMENT_3D('',#6293,#5053,#5054);
#4204=AXIS2_PLACEMENT_3D('',#6295,#5056,#5057);
#4205=AXIS2_PLACEMENT_3D('',#6299,#5060,#5061);
#4206=AXIS2_PLACEMENT_3D('',#6303,#5064,#5065);
#4207=AXIS2_PLACEMENT_3D('',#6304,#5066,#5067);
#4208=AXIS2_PLACEMENT_3D('',#6305,#5068,#5069);
#4209=AXIS2_PLACEMENT_3D('',#6306,#5070,#5071);
#4210=AXIS2_PLACEMENT_3D('',#6307,#5072,#5073);
#4211=AXIS2_PLACEMENT_3D('',#6309,#5074,#5075);
#4212=AXIS2_PLACEMENT_3D('',#6310,#5076,#5077);
#4213=AXIS2_PLACEMENT_3D('',#6312,#5078,#5079);
#4214=AXIS2_PLACEMENT_3D('',#6314,#5081,#5082);
#4215=AXIS2_PLACEMENT_3D('',#6316,#5083,#5084);
#4216=AXIS2_PLACEMENT_3D('',#6318,#5086,#5087);
#4217=AXIS2_PLACEMENT_3D('',#6320,#5088,#5089);
#4218=AXIS2_PLACEMENT_3D('',#6322,#5091,#5092);
#4219=AXIS2_PLACEMENT_3D('',#6324,#5093,#5094);
#4220=AXIS2_PLACEMENT_3D('',#6325,#5095,#5096);
#4221=AXIS2_PLACEMENT_3D('',#6327,#5097,#5098);
#4222=AXIS2_PLACEMENT_3D('',#6329,#5100,#5101);
#4223=AXIS2_PLACEMENT_3D('',#6331,#5102,#5103);
#4224=AXIS2_PLACEMENT_3D('',#6333,#5105,#5106);
#4225=AXIS2_PLACEMENT_3D('',#6335,#5107,#5108);
#4226=AXIS2_PLACEMENT_3D('',#6337,#5110,#5111);
#4227=AXIS2_PLACEMENT_3D('',#6338,#5112,#5113);
#4228=AXIS2_PLACEMENT_3D('',#6347,#5118,#5119);
#4229=AXIS2_PLACEMENT_3D('',#6353,#5123,#5124);
#4230=AXIS2_PLACEMENT_3D('',#6359,#5128,#5129);
#4231=AXIS2_PLACEMENT_3D('',#6365,#5133,#5134);
#4232=AXIS2_PLACEMENT_3D('',#6371,#5138,#5139);
#4233=AXIS2_PLACEMENT_3D('',#6374,#5142,#5143);
#4234=AXIS2_PLACEMENT_3D('',#6375,#5144,#5145);
#4235=AXIS2_PLACEMENT_3D('',#6376,#5146,#5147);
#4236=AXIS2_PLACEMENT_3D('',#6377,#5148,#5149);
#4237=AXIS2_PLACEMENT_3D('',#6389,#5151,#5152);
#4238=AXIS2_PLACEMENT_3D('',#6405,#5153,#5154);
#4239=AXIS2_PLACEMENT_3D('',#6407,#5155,#5156);
#4240=AXIS2_PLACEMENT_3D('',#6433,#5158,#5159);
#4241=AXIS2_PLACEMENT_3D('',#6436,#5162,#5163);
#4242=AXIS2_PLACEMENT_3D('',#6438,#5165,#5166);
#4243=AXIS2_PLACEMENT_3D('',#6440,#5168,#5169);
#4244=AXIS2_PLACEMENT_3D('',#6442,#5170,#5171);
#4245=AXIS2_PLACEMENT_3D('',#6445,#5173,#5174);
#4246=AXIS2_PLACEMENT_3D('',#6446,#5175,#5176);
#4247=AXIS2_PLACEMENT_3D('',#6448,#5178,#5179);
#4248=AXIS2_PLACEMENT_3D('',#6450,#5181,#5182);
#4249=AXIS2_PLACEMENT_3D('',#6451,#5183,#5184);
#4250=AXIS2_PLACEMENT_3D('',#6452,#5185,#5186);
#4251=AXIS2_PLACEMENT_3D('',#6453,#5187,#5188);
#4252=AXIS2_PLACEMENT_3D('',#6454,#5189,#5190);
#4253=AXIS2_PLACEMENT_3D('',#6456,#5191,#5192);
#4254=AXIS2_PLACEMENT_3D('',#6459,#5194,#5195);
#4255=AXIS2_PLACEMENT_3D('',#6460,#5196,#5197);
#4256=AXIS2_PLACEMENT_3D('',#6463,#5199,#5200);
#4257=AXIS2_PLACEMENT_3D('',#6464,#5201,#5202);
#4258=AXIS2_PLACEMENT_3D('',#6466,#5203,#5204);
#4259=AXIS2_PLACEMENT_3D('',#6467,#5205,#5206);
#4260=AXIS2_PLACEMENT_3D('',#6470,#5208,#5209);
#4261=AXIS2_PLACEMENT_3D('',#6471,#5210,#5211);
#4262=AXIS2_PLACEMENT_3D('',#6472,#5212,#5213);
#4263=AXIS2_PLACEMENT_3D('',#6473,#5214,#5215);
#4264=AXIS2_PLACEMENT_3D('',#6474,#5216,#5217);
#4265=AXIS2_PLACEMENT_3D('',#6475,#5218,#5219);
#4266=AXIS2_PLACEMENT_3D('',#6476,#5220,#5221);
#4267=AXIS2_PLACEMENT_3D('',#6477,#5222,#5223);
#4268=AXIS2_PLACEMENT_3D('',#6478,#5224,#5225);
#4269=AXIS2_PLACEMENT_3D('',#6479,#5226,#5227);
#4270=AXIS2_PLACEMENT_3D('',#6480,#5228,#5229);
#4271=AXIS2_PLACEMENT_3D('',#6481,#5230,#5231);
#4272=AXIS2_PLACEMENT_3D('',#6482,#5232,#5233);
#4273=AXIS2_PLACEMENT_3D('',#6483,#5234,#5235);
#4274=AXIS2_PLACEMENT_3D('',#6484,#5236,#5237);
#4275=AXIS2_PLACEMENT_3D('',#6485,#5238,#5239);
#4276=AXIS2_PLACEMENT_3D('',#6486,#5240,#5241);
#4277=AXIS2_PLACEMENT_3D('',#6487,#5242,#5243);
#4278=AXIS2_PLACEMENT_3D('',#6488,#5244,#5245);
#4279=AXIS2_PLACEMENT_3D('',#6489,#5246,#5247);
#4280=AXIS2_PLACEMENT_3D('',#6490,#5248,#5249);
#4281=AXIS2_PLACEMENT_3D('',#6491,#5250,#5251);
#4282=AXIS2_PLACEMENT_3D('',#6492,#5252,#5253);
#4283=AXIS2_PLACEMENT_3D('',#6493,#5254,#5255);
#4284=AXIS2_PLACEMENT_3D('',#6494,#5256,#5257);
#4285=AXIS2_PLACEMENT_3D('',#6495,#5258,#5259);
#4286=AXIS2_PLACEMENT_3D('',#6496,#5260,#5261);
#4287=AXIS2_PLACEMENT_3D('',#6497,#5262,#5263);
#4288=AXIS2_PLACEMENT_3D('',#6498,#5264,#5265);
#4289=AXIS2_PLACEMENT_3D('',#6499,#5266,#5267);
#4290=AXIS2_PLACEMENT_3D('',#6500,#5268,#5269);
#4291=AXIS2_PLACEMENT_3D('',#6501,#5270,#5271);
#4292=AXIS2_PLACEMENT_3D('',#6502,#5272,#5273);
#4293=AXIS2_PLACEMENT_3D('',#6503,#5274,#5275);
#4294=AXIS2_PLACEMENT_3D('',#6504,#5276,#5277);
#4295=AXIS2_PLACEMENT_3D('',#6506,#5278,#5279);
#4296=AXIS2_PLACEMENT_3D('',#6507,#5280,#5281);
#4297=AXIS2_PLACEMENT_3D('',#6509,#5282,#5283);
#4298=AXIS2_PLACEMENT_3D('',#6511,#5285,#5286);
#4299=AXIS2_PLACEMENT_3D('',#6513,#5287,#5288);
#4300=AXIS2_PLACEMENT_3D('',#6515,#5290,#5291);
#4301=AXIS2_PLACEMENT_3D('',#6517,#5292,#5293);
#4302=AXIS2_PLACEMENT_3D('',#6519,#5295,#5296);
#4303=AXIS2_PLACEMENT_3D('',#6521,#5297,#5298);
#4304=AXIS2_PLACEMENT_3D('',#6522,#5299,#5300);
#4305=AXIS2_PLACEMENT_3D('',#6524,#5301,#5302);
#4306=AXIS2_PLACEMENT_3D('',#6526,#5304,#5305);
#4307=AXIS2_PLACEMENT_3D('',#6528,#5306,#5307);
#4308=AXIS2_PLACEMENT_3D('',#6530,#5309,#5310);
#4309=AXIS2_PLACEMENT_3D('',#6532,#5311,#5312);
#4310=AXIS2_PLACEMENT_3D('',#6534,#5314,#5315);
#4311=AXIS2_PLACEMENT_3D('',#6535,#5316,#5317);
#4312=AXIS2_PLACEMENT_3D('',#6544,#5322,#5323);
#4313=AXIS2_PLACEMENT_3D('',#6550,#5327,#5328);
#4314=AXIS2_PLACEMENT_3D('',#6556,#5332,#5333);
#4315=AXIS2_PLACEMENT_3D('',#6562,#5337,#5338);
#4316=AXIS2_PLACEMENT_3D('',#6568,#5342,#5343);
#4317=AXIS2_PLACEMENT_3D('',#6571,#5346,#5347);
#4318=AXIS2_PLACEMENT_3D('',#6572,#5348,#5349);
#4319=AXIS2_PLACEMENT_3D('',#6573,#5350,#5351);
#4320=AXIS2_PLACEMENT_3D('',#6574,#5352,#5353);
#4321=AXIS2_PLACEMENT_3D('',#6586,#5355,#5356);
#4322=AXIS2_PLACEMENT_3D('',#6602,#5357,#5358);
#4323=AXIS2_PLACEMENT_3D('',#6604,#5359,#5360);
#4324=AXIS2_PLACEMENT_3D('',#6630,#5362,#5363);
#4325=AXIS2_PLACEMENT_3D('',#6633,#5366,#5367);
#4326=AXIS2_PLACEMENT_3D('',#6635,#5369,#5370);
#4327=AXIS2_PLACEMENT_3D('',#6637,#5372,#5373);
#4328=AXIS2_PLACEMENT_3D('',#6639,#5374,#5375);
#4329=AXIS2_PLACEMENT_3D('',#6642,#5377,#5378);
#4330=AXIS2_PLACEMENT_3D('',#6643,#5379,#5380);
#4331=AXIS2_PLACEMENT_3D('',#6645,#5382,#5383);
#4332=AXIS2_PLACEMENT_3D('',#6647,#5385,#5386);
#4333=AXIS2_PLACEMENT_3D('',#6648,#5387,#5388);
#4334=AXIS2_PLACEMENT_3D('',#6649,#5389,#5390);
#4335=AXIS2_PLACEMENT_3D('',#6650,#5391,#5392);
#4336=AXIS2_PLACEMENT_3D('',#6651,#5393,#5394);
#4337=AXIS2_PLACEMENT_3D('',#6652,#5395,#5396);
#4338=AXIS2_PLACEMENT_3D('',#6653,#5397,#5398);
#4339=AXIS2_PLACEMENT_3D('',#6654,#5399,#5400);
#4340=AXIS2_PLACEMENT_3D('',#6655,#5401,#5402);
#4341=AXIS2_PLACEMENT_3D('',#6656,#5403,#5404);
#4342=AXIS2_PLACEMENT_3D('',#6657,#5405,#5406);
#4343=AXIS2_PLACEMENT_3D('',#6658,#5407,#5408);
#4344=AXIS2_PLACEMENT_3D('',#6659,#5409,#5410);
#4345=AXIS2_PLACEMENT_3D('',#6660,#5411,#5412);
#4346=AXIS2_PLACEMENT_3D('',#6661,#5413,#5414);
#4347=AXIS2_PLACEMENT_3D('',#6662,#5415,#5416);
#4348=AXIS2_PLACEMENT_3D('',#6663,#5417,#5418);
#4349=AXIS2_PLACEMENT_3D('',#6664,#5419,#5420);
#4350=AXIS2_PLACEMENT_3D('',#6665,#5421,#5422);
#4351=AXIS2_PLACEMENT_3D('',#6666,#5423,#5424);
#4352=AXIS2_PLACEMENT_3D('',#6668,#5425,#5426);
#4353=AXIS2_PLACEMENT_3D('',#6671,#5428,#5429);
#4354=AXIS2_PLACEMENT_3D('',#6672,#5430,#5431);
#4355=AXIS2_PLACEMENT_3D('',#6681,#5436,#5437);
#4356=AXIS2_PLACEMENT_3D('',#6687,#5441,#5442);
#4357=AXIS2_PLACEMENT_3D('',#6693,#5446,#5447);
#4358=AXIS2_PLACEMENT_3D('',#6696,#5450,#5451);
#4359=AXIS2_PLACEMENT_3D('',#6697,#5452,#5453);
#4360=AXIS2_PLACEMENT_3D('',#6698,#5454,#5455);
#4361=AXIS2_PLACEMENT_3D('',#6699,#5456,#5457);
#4362=AXIS2_PLACEMENT_3D('',#6700,#5458,#5459);
#4363=AXIS2_PLACEMENT_3D('',#6701,#5460,#5461);
#4364=DIRECTION('axis',(0.,0.,1.));
#4365=DIRECTION('refdir',(1.,0.,0.));
#4366=DIRECTION('axis',(0.,0.,1.));
#4367=DIRECTION('refdir',(1.,0.,0.));
#4368=DIRECTION('axis',(0.,0.,1.));
#4369=DIRECTION('refdir',(1.,0.,0.));
#4370=DIRECTION('center_axis',(0.,1.,0.));
#4371=DIRECTION('ref_axis',(1.,0.,0.));
#4372=DIRECTION('center_axis',(0.,1.,0.));
#4373=DIRECTION('ref_axis',(1.,0.,0.));
#4374=DIRECTION('',(0.,1.,0.));
#4375=DIRECTION('center_axis',(0.,-1.,0.));
#4376=DIRECTION('ref_axis',(1.,0.,0.));
#4377=DIRECTION('center_axis',(0.,1.,0.));
#4378=DIRECTION('ref_axis',(1.,0.,0.));
#4379=DIRECTION('center_axis',(0.,1.,0.));
#4380=DIRECTION('ref_axis',(1.,0.,0.));
#4381=DIRECTION('',(0.,1.,0.));
#4382=DIRECTION('center_axis',(0.,-1.,0.));
#4383=DIRECTION('ref_axis',(1.,0.,0.));
#4384=DIRECTION('center_axis',(0.,1.,0.));
#4385=DIRECTION('ref_axis',(-1.,0.,0.));
#4386=DIRECTION('',(-1.,0.,0.));
#4387=DIRECTION('',(0.,0.,1.));
#4388=DIRECTION('',(-1.,0.,0.));
#4389=DIRECTION('',(0.,0.,1.));
#4390=DIRECTION('center_axis',(1.,0.,0.));
#4391=DIRECTION('ref_axis',(0.,1.,0.));
#4392=DIRECTION('',(0.,1.,0.));
#4393=DIRECTION('',(0.,1.,0.));
#4394=DIRECTION('',(0.,0.,1.));
#4395=DIRECTION('center_axis',(0.,-1.,0.));
#4396=DIRECTION('ref_axis',(1.,0.,0.));
#4397=DIRECTION('',(1.,0.,0.));
#4398=DIRECTION('',(1.,0.,0.));
#4399=DIRECTION('',(0.,0.,1.));
#4400=DIRECTION('center_axis',(-1.,0.,0.));
#4401=DIRECTION('ref_axis',(0.,-1.,0.));
#4402=DIRECTION('',(0.,-1.,0.));
#4403=DIRECTION('',(0.,-1.,0.));
#4404=DIRECTION('center_axis',(0.,0.,1.));
#4405=DIRECTION('ref_axis',(1.,0.,0.));
#4406=DIRECTION('center_axis',(0.,0.,1.));
#4407=DIRECTION('ref_axis',(1.,0.,0.));
#4408=DIRECTION('axis',(0.,0.,1.));
#4409=DIRECTION('refdir',(1.,0.,0.));
#4410=DIRECTION('center_axis',(0.,0.,-1.));
#4411=DIRECTION('ref_axis',(0.,1.,0.));
#4412=DIRECTION('',(0.,1.,0.));
#4413=DIRECTION('',(1.,0.,0.));
#4414=DIRECTION('',(0.,-1.,0.));
#4415=DIRECTION('',(1.,0.,0.));
#4416=DIRECTION('center_axis',(0.,1.,-8.88178419700125E-16));
#4417=DIRECTION('ref_axis',(0.,8.88178419700125E-16,1.));
#4418=DIRECTION('',(0.,8.88178419700125E-16,1.));
#4419=DIRECTION('',(1.,0.,0.));
#4420=DIRECTION('',(0.,-8.88178419700125E-16,-1.));
#4421=DIRECTION('center_axis',(0.,-7.40148683083439E-16,-1.));
#4422=DIRECTION('ref_axis',(0.,1.,-7.40148683083439E-16));
#4423=DIRECTION('',(0.,1.,-7.40148683083439E-16));
#4424=DIRECTION('',(1.,0.,0.));
#4425=DIRECTION('',(0.,-1.,7.40148683083439E-16));
#4426=DIRECTION('center_axis',(0.,-0.707106781186547,-0.707106781186548));
#4427=DIRECTION('ref_axis',(0.,0.707106781186548,-0.707106781186547));
#4428=DIRECTION('',(0.,0.707106781186548,-0.707106781186547));
#4429=DIRECTION('',(1.,0.,0.));
#4430=DIRECTION('',(0.,-0.707106781186548,0.707106781186547));
#4431=DIRECTION('center_axis',(0.,-1.,2.77555756156289E-16));
#4432=DIRECTION('ref_axis',(0.,-2.77555756156289E-16,-1.));
#4433=DIRECTION('',(0.,-2.77555756156289E-16,-1.));
#4434=DIRECTION('',(1.,0.,0.));
#4435=DIRECTION('',(0.,2.77555756156289E-16,1.));
#4436=DIRECTION('center_axis',(0.,-0.707106781186547,0.707106781186548));
#4437=DIRECTION('ref_axis',(0.,-0.707106781186548,-0.707106781186547));
#4438=DIRECTION('',(0.,-0.707106781186548,-0.707106781186547));
#4439=DIRECTION('',(1.,0.,0.));
#4440=DIRECTION('',(0.,0.707106781186548,0.707106781186547));
#4441=DIRECTION('center_axis',(0.,7.40148683083438E-16,1.));
#4442=DIRECTION('ref_axis',(0.,-1.,7.40148683083438E-16));
#4443=DIRECTION('',(0.,-1.,7.40148683083438E-16));
#4444=DIRECTION('',(1.,0.,0.));
#4445=DIRECTION('',(0.,1.,-7.40148683083438E-16));
#4446=DIRECTION('center_axis',(0.,1.,-4.44089209850063E-16));
#4447=DIRECTION('ref_axis',(0.,4.44089209850063E-16,1.));
#4448=DIRECTION('',(0.,4.44089209850063E-16,1.));
#4449=DIRECTION('',(1.,0.,0.));
#4450=DIRECTION('',(0.,-4.44089209850063E-16,-1.));
#4451=DIRECTION('center_axis',(0.,2.41352831440251E-16,1.));
#4452=DIRECTION('ref_axis',(0.,-1.,2.41352831440251E-16));
#4453=DIRECTION('',(0.,-1.,2.41352831440251E-16));
#4454=DIRECTION('',(-1.,0.,0.));
#4455=DIRECTION('',(0.,1.,-2.41352831440251E-16));
#4456=DIRECTION('center_axis',(0.,-1.,2.41352831440251E-16));
#4457=DIRECTION('ref_axis',(0.,-2.41352831440251E-16,-1.));
#4458=DIRECTION('',(0.,-2.41352831440251E-16,-1.));
#4459=DIRECTION('',(1.,0.,0.));
#4460=DIRECTION('',(0.,2.41352831440251E-16,1.));
#4461=DIRECTION('',(1.,0.,0.));
#4462=DIRECTION('center_axis',(0.,0.,-1.));
#4463=DIRECTION('ref_axis',(0.,1.,0.));
#4464=DIRECTION('',(0.,1.,0.));
#4465=DIRECTION('',(1.,0.,0.));
#4466=DIRECTION('',(0.,-1.,0.));
#4467=DIRECTION('center_axis',(0.,-1.,0.));
#4468=DIRECTION('ref_axis',(0.,0.,-1.));
#4469=DIRECTION('',(0.,0.,-1.));
#4470=DIRECTION('',(1.,0.,0.));
#4471=DIRECTION('',(0.,0.,1.));
#4472=DIRECTION('center_axis',(0.,-0.707106781186547,0.707106781186548));
#4473=DIRECTION('ref_axis',(0.,-0.707106781186548,-0.707106781186547));
#4474=DIRECTION('',(0.,-0.707106781186548,-0.707106781186547));
#4475=DIRECTION('',(1.,0.,0.));
#4476=DIRECTION('',(0.,0.707106781186548,0.707106781186547));
#4477=DIRECTION('center_axis',(0.,0.,1.));
#4478=DIRECTION('ref_axis',(0.,-1.,0.));
#4479=DIRECTION('',(0.,-1.,0.));
#4480=DIRECTION('',(1.,0.,0.));
#4481=DIRECTION('',(0.,1.,0.));
#4482=DIRECTION('center_axis',(0.,0.707106781186548,0.707106781186547));
#4483=DIRECTION('ref_axis',(0.,-0.707106781186547,0.707106781186548));
#4484=DIRECTION('',(0.,-0.707106781186547,0.707106781186548));
#4485=DIRECTION('',(1.,0.,0.));
#4486=DIRECTION('',(0.,0.707106781186547,-0.707106781186548));
#4487=DIRECTION('center_axis',(0.,1.,0.));
#4488=DIRECTION('ref_axis',(0.,0.,1.));
#4489=DIRECTION('',(0.,0.,1.));
#4490=DIRECTION('',(1.,0.,0.));
#4491=DIRECTION('',(0.,0.,-1.));
#4492=DIRECTION('center_axis',(0.,0.,-1.));
#4493=DIRECTION('ref_axis',(0.,1.,0.));
#4494=DIRECTION('',(0.,1.,0.));
#4495=DIRECTION('',(1.,0.,0.));
#4496=DIRECTION('',(0.,-1.,0.));
#4497=DIRECTION('center_axis',(0.,1.,-2.41352831440251E-16));
#4498=DIRECTION('ref_axis',(0.,2.41352831440251E-16,1.));
#4499=DIRECTION('',(0.,2.41352831440251E-16,1.));
#4500=DIRECTION('',(-1.,0.,0.));
#4501=DIRECTION('',(0.,-2.41352831440251E-16,-1.));
#4502=DIRECTION('center_axis',(0.,0.,1.));
#4503=DIRECTION('ref_axis',(0.,-1.,0.));
#4504=DIRECTION('',(0.,-1.,0.));
#4505=DIRECTION('',(1.,0.,0.));
#4506=DIRECTION('',(0.,1.,0.));
#4507=DIRECTION('',(1.,0.,0.));
#4508=DIRECTION('center_axis',(0.,-1.,0.));
#4509=DIRECTION('ref_axis',(0.,0.,-1.));
#4510=DIRECTION('',(0.,0.,-1.));
#4511=DIRECTION('',(1.,0.,0.));
#4512=DIRECTION('',(0.,0.,1.));
#4513=DIRECTION('center_axis',(0.,0.,1.));
#4514=DIRECTION('ref_axis',(0.,-1.,0.));
#4515=DIRECTION('',(0.,-1.,0.));
#4516=DIRECTION('',(1.,0.,0.));
#4517=DIRECTION('',(0.,1.,0.));
#4518=DIRECTION('center_axis',(0.,0.707106781186548,0.707106781186548));
#4519=DIRECTION('ref_axis',(0.,-0.707106781186548,0.707106781186548));
#4520=DIRECTION('',(0.,-0.707106781186548,0.707106781186548));
#4521=DIRECTION('',(1.,0.,0.));
#4522=DIRECTION('',(0.,0.707106781186548,-0.707106781186548));
#4523=DIRECTION('center_axis',(0.,1.,0.));
#4524=DIRECTION('ref_axis',(0.,0.,1.));
#4525=DIRECTION('',(0.,0.,1.));
#4526=DIRECTION('',(1.,0.,0.));
#4527=DIRECTION('',(0.,0.,-1.));
#4528=DIRECTION('center_axis',(0.,0.707106781186548,-0.707106781186547));
#4529=DIRECTION('ref_axis',(0.,0.707106781186547,0.707106781186548));
#4530=DIRECTION('',(0.,0.707106781186547,0.707106781186548));
#4531=DIRECTION('',(1.,0.,0.));
#4532=DIRECTION('',(0.,-0.707106781186547,-0.707106781186548));
#4533=DIRECTION('center_axis',(0.,-7.40148683083438E-16,-1.));
#4534=DIRECTION('ref_axis',(0.,1.,-7.40148683083438E-16));
#4535=DIRECTION('',(0.,1.,-7.40148683083438E-16));
#4536=DIRECTION('',(1.,0.,0.));
#4537=DIRECTION('',(0.,-1.,7.40148683083438E-16));
#4538=DIRECTION('center_axis',(0.,-1.,0.));
#4539=DIRECTION('ref_axis',(0.,0.,-1.));
#4540=DIRECTION('',(0.,0.,-1.));
#4541=DIRECTION('',(1.,0.,0.));
#4542=DIRECTION('',(0.,0.,1.));
#4543=DIRECTION('center_axis',(0.,0.,-1.));
#4544=DIRECTION('ref_axis',(0.,1.,0.));
#4545=DIRECTION('',(0.,1.,0.));
#4546=DIRECTION('',(-1.,0.,0.));
#4547=DIRECTION('',(0.,-1.,0.));
#4548=DIRECTION('center_axis',(0.,1.,0.));
#4549=DIRECTION('ref_axis',(0.,0.,1.));
#4550=DIRECTION('',(0.,0.,1.));
#4551=DIRECTION('',(1.,0.,0.));
#4552=DIRECTION('',(0.,0.,-1.));
#4553=DIRECTION('',(1.,0.,0.));
#4554=DIRECTION('center_axis',(0.,0.,1.));
#4555=DIRECTION('ref_axis',(0.,-1.,0.));
#4556=DIRECTION('',(0.,-1.,0.));
#4557=DIRECTION('',(1.,0.,0.));
#4558=DIRECTION('',(0.,1.,0.));
#4559=DIRECTION('center_axis',(0.,1.,0.));
#4560=DIRECTION('ref_axis',(0.,0.,1.));
#4561=DIRECTION('',(0.,0.,1.));
#4562=DIRECTION('',(1.,0.,0.));
#4563=DIRECTION('',(0.,0.,-1.));
#4564=DIRECTION('center_axis',(0.,0.707106781186547,-0.707106781186548));
#4565=DIRECTION('ref_axis',(0.,0.707106781186548,0.707106781186547));
#4566=DIRECTION('',(0.,0.707106781186548,0.707106781186547));
#4567=DIRECTION('',(1.,0.,0.));
#4568=DIRECTION('',(0.,-0.707106781186548,-0.707106781186547));
#4569=DIRECTION('center_axis',(0.,0.,-1.));
#4570=DIRECTION('ref_axis',(0.,1.,0.));
#4571=DIRECTION('',(0.,1.,0.));
#4572=DIRECTION('',(1.,0.,0.));
#4573=DIRECTION('',(0.,-1.,0.));
#4574=DIRECTION('center_axis',(0.,-0.707106781186547,-0.707106781186548));
#4575=DIRECTION('ref_axis',(0.,0.707106781186548,-0.707106781186547));
#4576=DIRECTION('',(0.,0.707106781186548,-0.707106781186547));
#4577=DIRECTION('',(1.,0.,0.));
#4578=DIRECTION('',(0.,-0.707106781186548,0.707106781186547));
#4579=DIRECTION('center_axis',(0.,-1.,0.));
#4580=DIRECTION('ref_axis',(0.,0.,-1.));
#4581=DIRECTION('',(0.,0.,-1.));
#4582=DIRECTION('',(1.,0.,0.));
#4583=DIRECTION('',(0.,0.,1.));
#4584=DIRECTION('center_axis',(0.,0.,1.));
#4585=DIRECTION('ref_axis',(0.,-1.,0.));
#4586=DIRECTION('',(0.,-1.,0.));
#4587=DIRECTION('',(1.,0.,0.));
#4588=DIRECTION('',(0.,1.,0.));
#4589=DIRECTION('center_axis',(0.,-1.,0.));
#4590=DIRECTION('ref_axis',(0.,0.,-1.));
#4591=DIRECTION('',(0.,0.,-1.));
#4592=DIRECTION('',(-1.,0.,0.));
#4593=DIRECTION('',(0.,0.,1.));
#4594=DIRECTION('center_axis',(1.,0.,0.));
#4595=DIRECTION('ref_axis',(0.,0.,-1.));
#4596=DIRECTION('center_axis',(1.,0.,0.));
#4597=DIRECTION('ref_axis',(0.,0.,-1.));
#4598=DIRECTION('',(1.,0.,0.));
#4599=DIRECTION('center_axis',(-1.,0.,0.));
#4600=DIRECTION('ref_axis',(0.,0.,-1.));
#4601=DIRECTION('center_axis',(0.,1.,0.));
#4602=DIRECTION('ref_axis',(0.,0.,1.));
#4603=DIRECTION('',(0.,0.,1.));
#4604=DIRECTION('',(1.,0.,0.));
#4605=DIRECTION('',(0.,0.,1.));
#4606=DIRECTION('center_axis',(0.,1.,0.));
#4607=DIRECTION('ref_axis',(0.,0.,1.));
#4608=DIRECTION('',(0.,0.,1.));
#4609=DIRECTION('',(1.,0.,0.));
#4610=DIRECTION('',(0.,0.,1.));
#4611=DIRECTION('center_axis',(0.,0.,-1.));
#4612=DIRECTION('ref_axis',(0.,1.,0.));
#4613=DIRECTION('',(0.,1.,0.));
#4614=DIRECTION('',(0.,1.,0.));
#4615=DIRECTION('center_axis',(0.,0.,-1.));
#4616=DIRECTION('ref_axis',(0.,1.,0.));
#4617=DIRECTION('',(0.,1.,0.));
#4618=DIRECTION('',(1.,0.,0.));
#4619=DIRECTION('',(0.,1.,0.));
#4620=DIRECTION('center_axis',(0.,-1.,0.));
#4621=DIRECTION('ref_axis',(0.,0.,-1.));
#4622=DIRECTION('',(0.,0.,-1.));
#4623=DIRECTION('',(0.,0.,-1.));
#4624=DIRECTION('center_axis',(0.,-1.,0.));
#4625=DIRECTION('ref_axis',(0.,0.,-1.));
#4626=DIRECTION('',(0.,0.,-1.));
#4627=DIRECTION('',(1.,0.,0.));
#4628=DIRECTION('',(0.,0.,-1.));
#4629=DIRECTION('center_axis',(0.,0.,1.));
#4630=DIRECTION('ref_axis',(0.,-1.,0.));
#4631=DIRECTION('',(0.,-1.,0.));
#4632=DIRECTION('',(0.,-1.,0.));
#4633=DIRECTION('center_axis',(0.,0.,1.));
#4634=DIRECTION('ref_axis',(0.,-1.,0.));
#4635=DIRECTION('',(0.,-1.,0.));
#4636=DIRECTION('',(0.,-1.,0.));
#4637=DIRECTION('center_axis',(1.,0.,0.));
#4638=DIRECTION('ref_axis',(0.,0.,-1.));
#4639=DIRECTION('center_axis',(1.,0.,0.));
#4640=DIRECTION('ref_axis',(0.,0.,-1.));
#4641=DIRECTION('axis',(0.,0.,1.));
#4642=DIRECTION('refdir',(1.,0.,0.));
#4643=DIRECTION('center_axis',(0.,1.,0.));
#4644=DIRECTION('ref_axis',(1.,0.,0.));
#4645=DIRECTION('center_axis',(0.,1.,0.));
#4646=DIRECTION('ref_axis',(1.,0.,0.));
#4647=DIRECTION('',(0.,1.,0.));
#4648=DIRECTION('center_axis',(0.,-1.,0.));
#4649=DIRECTION('ref_axis',(1.,0.,0.));
#4650=DIRECTION('center_axis',(0.,1.,0.));
#4651=DIRECTION('ref_axis',(1.,0.,0.));
#4652=DIRECTION('center_axis',(0.,1.,0.));
#4653=DIRECTION('ref_axis',(1.,0.,0.));
#4654=DIRECTION('',(0.,1.,0.));
#4655=DIRECTION('center_axis',(0.,-1.,0.));
#4656=DIRECTION('ref_axis',(1.,0.,0.));
#4657=DIRECTION('center_axis',(0.,0.,1.));
#4658=DIRECTION('ref_axis',(1.,0.,0.));
#4659=DIRECTION('center_axis',(0.,0.,1.));
#4660=DIRECTION('ref_axis',(1.,0.,0.));
#4661=DIRECTION('',(0.,0.,1.));
#4662=DIRECTION('center_axis',(0.,0.,-1.));
#4663=DIRECTION('ref_axis',(1.,0.,0.));
#4664=DIRECTION('center_axis',(0.,0.,1.));
#4665=DIRECTION('ref_axis',(1.,0.,0.));
#4666=DIRECTION('center_axis',(0.,0.,1.));
#4667=DIRECTION('ref_axis',(1.,0.,0.));
#4668=DIRECTION('',(0.,0.,1.));
#4669=DIRECTION('center_axis',(0.,0.,-1.));
#4670=DIRECTION('ref_axis',(1.,0.,0.));
#4671=DIRECTION('center_axis',(-1.,0.,0.));
#4672=DIRECTION('ref_axis',(0.,-1.,0.));
#4673=DIRECTION('',(0.,0.,1.));
#4674=DIRECTION('',(0.,-1.,0.));
#4675=DIRECTION('',(0.,0.,1.));
#4676=DIRECTION('',(0.,-1.,0.));
#4677=DIRECTION('center_axis',(0.,1.,0.));
#4678=DIRECTION('ref_axis',(-1.,0.,0.));
#4679=DIRECTION('',(0.,0.,-1.));
#4680=DIRECTION('',(-1.,0.,0.));
#4681=DIRECTION('',(-1.,0.,0.));
#4682=DIRECTION('center_axis',(0.,-1.,0.));
#4683=DIRECTION('ref_axis',(1.,0.,0.));
#4684=DIRECTION('',(-1.,0.,0.));
#4685=DIRECTION('',(1.,0.,0.));
#4686=DIRECTION('',(0.,0.,1.));
#4687=DIRECTION('',(1.,0.,0.));
#4688=DIRECTION('',(0.,0.,1.));
#4689=DIRECTION('',(1.,0.,0.));
#4690=DIRECTION('',(0.,0.,1.));
#4691=DIRECTION('center_axis',(0.,0.,1.));
#4692=DIRECTION('ref_axis',(1.,0.,0.));
#4693=DIRECTION('',(0.,0.,-1.));
#4694=DIRECTION('center_axis',(0.,0.,1.));
#4695=DIRECTION('ref_axis',(1.,0.,0.));
#4696=DIRECTION('center_axis',(0.,0.,1.));
#4697=DIRECTION('ref_axis',(1.,0.,0.));
#4698=DIRECTION('center_axis',(0.,0.,1.));
#4699=DIRECTION('ref_axis',(1.,0.,0.));
#4700=DIRECTION('',(0.,1.,0.));
#4701=DIRECTION('center_axis',(1.,0.,0.));
#4702=DIRECTION('ref_axis',(0.,1.,0.));
#4703=DIRECTION('',(0.,-1.,0.));
#4704=DIRECTION('',(0.,0.,-1.));
#4705=DIRECTION('',(0.,1.,0.));
#4706=DIRECTION('',(0.,0.,1.));
#4707=DIRECTION('',(0.,1.,0.));
#4708=DIRECTION('center_axis',(0.,0.,1.));
#4709=DIRECTION('ref_axis',(1.,0.,0.));
#4710=DIRECTION('center_axis',(0.,0.,1.));
#4711=DIRECTION('ref_axis',(1.,0.,0.));
#4712=DIRECTION('center_axis',(0.,0.,1.));
#4713=DIRECTION('ref_axis',(1.,0.,0.));
#4714=DIRECTION('center_axis',(0.,0.,1.));
#4715=DIRECTION('ref_axis',(1.,0.,0.));
#4716=DIRECTION('center_axis',(0.,0.,1.));
#4717=DIRECTION('ref_axis',(1.,0.,0.));
#4718=DIRECTION('',(0.,-1.,0.));
#4719=DIRECTION('',(-1.,0.,0.));
#4720=DIRECTION('center_axis',(0.,1.,0.));
#4721=DIRECTION('ref_axis',(-1.,0.,0.));
#4722=DIRECTION('',(0.,0.,1.));
#4723=DIRECTION('',(-1.,0.,0.));
#4724=DIRECTION('center_axis',(-1.,0.,0.));
#4725=DIRECTION('ref_axis',(0.,-1.,0.));
#4726=DIRECTION('',(0.,-1.,0.));
#4727=DIRECTION('center_axis',(0.,0.,1.));
#4728=DIRECTION('ref_axis',(1.,0.,0.));
#4729=DIRECTION('axis',(0.,0.,1.));
#4730=DIRECTION('refdir',(1.,0.,0.));
#4731=DIRECTION('center_axis',(1.,0.,0.));
#4732=DIRECTION('ref_axis',(0.,0.,-1.));
#4733=DIRECTION('',(1.,0.,0.));
#4734=DIRECTION('center_axis',(0.,1.,0.));
#4735=DIRECTION('ref_axis',(0.,0.,1.));
#4736=DIRECTION('center_axis',(0.,-1.,0.));
#4737=DIRECTION('ref_axis',(1.,0.,0.));
#4738=DIRECTION('center_axis',(0.,-1.,0.));
#4739=DIRECTION('ref_axis',(1.,0.,0.));
#4740=DIRECTION('center_axis',(0.,-1.,0.));
#4741=DIRECTION('ref_axis',(1.,0.,0.));
#4742=DIRECTION('',(0.707106781186547,0.707106781186548,8.65956056235493E-17));
#4743=DIRECTION('center_axis',(0.,-1.,0.));
#4744=DIRECTION('ref_axis',(1.,0.,0.));
#4745=DIRECTION('center_axis',(0.,-1.,0.));
#4746=DIRECTION('ref_axis',(1.,0.,0.));
#4747=DIRECTION('',(0.,1.,0.));
#4748=DIRECTION('center_axis',(0.,-1.,0.));
#4749=DIRECTION('ref_axis',(0.,0.,-1.));
#4750=DIRECTION('center_axis',(0.,-1.,0.));
#4751=DIRECTION('ref_axis',(1.,0.,0.));
#4752=DIRECTION('center_axis',(0.,-1.,0.));
#4753=DIRECTION('ref_axis',(1.,0.,0.));
#4754=DIRECTION('center_axis',(0.,-1.,0.));
#4755=DIRECTION('ref_axis',(1.,0.,0.));
#4756=DIRECTION('',(0.,1.,0.));
#4757=DIRECTION('',(0.,1.,0.));
#4758=DIRECTION('center_axis',(0.,1.,0.));
#4759=DIRECTION('ref_axis',(1.,0.,0.));
#4760=DIRECTION('center_axis',(0.,-1.,0.));
#4761=DIRECTION('ref_axis',(1.,0.,0.));
#4762=DIRECTION('',(-0.707106781186548,0.707106781186547,-8.65956056235494E-17));
#4763=DIRECTION('center_axis',(0.,-1.,0.));
#4764=DIRECTION('ref_axis',(0.,0.,-1.));
#4765=DIRECTION('axis',(0.,0.,1.));
#4766=DIRECTION('refdir',(1.,0.,0.));
#4767=DIRECTION('center_axis',(0.,1.,0.));
#4768=DIRECTION('ref_axis',(1.,0.,0.));
#4769=DIRECTION('center_axis',(0.,-1.,0.));
#4770=DIRECTION('ref_axis',(1.,0.,0.));
#4771=DIRECTION('',(0.,-1.,0.));
#4772=DIRECTION('center_axis',(0.,-1.,0.));
#4773=DIRECTION('ref_axis',(1.,0.,0.));
#4774=DIRECTION('center_axis',(0.,1.,0.));
#4775=DIRECTION('ref_axis',(1.,0.,0.));
#4776=DIRECTION('center_axis',(0.,1.,0.));
#4777=DIRECTION('ref_axis',(1.,0.,0.));
#4778=DIRECTION('',(0.,-1.,0.));
#4779=DIRECTION('center_axis',(0.,1.,0.));
#4780=DIRECTION('ref_axis',(1.,0.,0.));
#4781=DIRECTION('center_axis',(0.,1.,0.));
#4782=DIRECTION('ref_axis',(1.,0.,0.));
#4783=DIRECTION('center_axis',(0.,1.,0.));
#4784=DIRECTION('ref_axis',(1.,0.,0.));
#4785=DIRECTION('axis',(0.,0.,1.));
#4786=DIRECTION('refdir',(1.,0.,0.));
#4787=DIRECTION('center_axis',(-1.,0.,0.));
#4788=DIRECTION('ref_axis',(0.,0.,1.));
#4789=DIRECTION('center_axis',(0.,-1.,1.38777878078145E-16));
#4790=DIRECTION('ref_axis',(0.,-1.38777878078145E-16,-1.));
#4791=DIRECTION('center_axis',(1.,0.,0.));
#4792=DIRECTION('ref_axis',(0.,0.,1.));
#4793=DIRECTION('center_axis',(0.,1.,0.));
#4794=DIRECTION('ref_axis',(1.,0.,0.));
#4795=DIRECTION('center_axis',(0.,-1.,0.));
#4796=DIRECTION('ref_axis',(1.,0.,0.));
#4797=DIRECTION('',(0.,0.,1.));
#4798=DIRECTION('center_axis',(1.,0.,0.));
#4799=DIRECTION('ref_axis',(0.,0.,1.));
#4800=DIRECTION('',(0.,-1.,0.));
#4801=DIRECTION('',(0.,0.,1.));
#4802=DIRECTION('',(0.,-1.,0.));
#4803=DIRECTION('center_axis',(0.,-1.,0.));
#4804=DIRECTION('ref_axis',(1.,0.,0.));
#4805=DIRECTION('center_axis',(0.,-1.,0.));
#4806=DIRECTION('ref_axis',(1.,0.,0.));
#4807=DIRECTION('',(0.,1.,0.));
#4808=DIRECTION('center_axis',(0.,-1.,0.));
#4809=DIRECTION('ref_axis',(1.,0.,0.));
#4810=DIRECTION('center_axis',(0.,1.,0.));
#4811=DIRECTION('ref_axis',(1.,0.,0.));
#4812=DIRECTION('axis',(0.,0.,1.));
#4813=DIRECTION('refdir',(1.,0.,0.));
#4814=DIRECTION('center_axis',(0.,-0.707106781186548,-0.707106781186548));
#4815=DIRECTION('ref_axis',(-1.,0.,0.));
#4816=DIRECTION('',(0.,-0.707106781186548,0.707106781186548));
#4817=DIRECTION('',(-1.,0.,0.));
#4818=DIRECTION('',(0.,0.707106781186548,-0.707106781186548));
#4819=DIRECTION('',(1.,0.,0.));
#4820=DIRECTION('center_axis',(0.,0.707106781186548,0.707106781186548));
#4821=DIRECTION('ref_axis',(0.,0.707106781186547,-0.707106781186547));
#4822=DIRECTION('',(1.,0.,0.));
#4823=DIRECTION('center_axis',(0.,0.,1.));
#4824=DIRECTION('ref_axis',(1.,0.,0.));
#4825=DIRECTION('center_axis',(0.,0.,-1.));
#4826=DIRECTION('ref_axis',(1.,0.,0.));
#4827=DIRECTION('',(0.,0.,1.));
#4828=DIRECTION('center_axis',(0.,0.,-1.));
#4829=DIRECTION('ref_axis',(1.,0.,0.));
#4830=DIRECTION('center_axis',(0.,0.,-1.));
#4831=DIRECTION('ref_axis',(1.,0.,0.));
#4832=DIRECTION('center_axis',(0.,-0.707106781186548,0.707106781186548));
#4833=DIRECTION('ref_axis',(0.,0.707106781186547,0.707106781186547));
#4834=DIRECTION('center_axis',(0.,0.,-1.));
#4835=DIRECTION('ref_axis',(1.,0.,0.));
#4836=DIRECTION('center_axis',(0.,0.,1.));
#4837=DIRECTION('ref_axis',(1.,0.,0.));
#4838=DIRECTION('',(0.,-1.,0.));
#4839=DIRECTION('',(-1.,0.,0.));
#4840=DIRECTION('center_axis',(0.,0.,1.));
#4841=DIRECTION('ref_axis',(1.,0.,0.));
#4842=DIRECTION('',(-1.,0.,0.));
#4843=DIRECTION('',(0.,1.,0.));
#4844=DIRECTION('center_axis',(0.,0.707106781186548,-0.707106781186548));
#4845=DIRECTION('ref_axis',(-1.,0.,0.));
#4846=DIRECTION('',(0.,0.707106781186548,0.707106781186548));
#4847=DIRECTION('',(1.,0.,0.));
#4848=DIRECTION('',(0.,-0.707106781186548,-0.707106781186548));
#4849=DIRECTION('center_axis',(1.,0.,0.));
#4850=DIRECTION('ref_axis',(0.,1.,0.));
#4851=DIRECTION('',(0.,0.,1.));
#4852=DIRECTION('',(0.,1.,0.));
#4853=DIRECTION('',(0.,0.,1.));
#4854=DIRECTION('center_axis',(0.,1.,0.));
#4855=DIRECTION('ref_axis',(-1.,0.,0.));
#4856=DIRECTION('',(0.,0.,1.));
#4857=DIRECTION('',(-1.,0.,0.));
#4858=DIRECTION('center_axis',(0.,-1.,0.));
#4859=DIRECTION('ref_axis',(1.,0.,0.));
#4860=DIRECTION('',(1.,0.,0.));
#4861=DIRECTION('',(0.,0.,1.));
#4862=DIRECTION('center_axis',(-1.,0.,0.));
#4863=DIRECTION('ref_axis',(0.,-1.,0.));
#4864=DIRECTION('',(0.,-1.,0.));
#4865=DIRECTION('center_axis',(0.,0.,1.));
#4866=DIRECTION('ref_axis',(1.,0.,0.));
#4867=DIRECTION('axis',(0.,0.,1.));
#4868=DIRECTION('refdir',(1.,0.,0.));
#4869=DIRECTION('center_axis',(0.866025403784439,0.,-0.5));
#4870=DIRECTION('ref_axis',(0.5,0.,0.866025403784439));
#4871=DIRECTION('',(-0.5,0.,-0.866025403784439));
#4872=DIRECTION('',(0.,-1.,0.));
#4873=DIRECTION('',(0.5,0.,0.866025403784439));
#4874=DIRECTION('',(0.,-1.,0.));
#4875=DIRECTION('center_axis',(1.20185167898973E-16,0.,-1.));
#4876=DIRECTION('ref_axis',(1.,0.,1.20185167898973E-16));
#4877=DIRECTION('',(-1.,0.,-1.20185167898973E-16));
#4878=DIRECTION('',(0.,-1.,0.));
#4879=DIRECTION('',(1.,0.,1.20185167898973E-16));
#4880=DIRECTION('center_axis',(-0.866025403784439,0.,-0.5));
#4881=DIRECTION('ref_axis',(0.5,0.,-0.866025403784439));
#4882=DIRECTION('',(-0.5,0.,0.866025403784439));
#4883=DIRECTION('',(0.,-1.,0.));
#4884=DIRECTION('',(0.5,0.,-0.866025403784439));
#4885=DIRECTION('center_axis',(-0.866025403784439,0.,0.5));
#4886=DIRECTION('ref_axis',(-0.5,0.,-0.866025403784439));
#4887=DIRECTION('',(0.5,0.,0.866025403784439));
#4888=DIRECTION('',(0.,-1.,0.));
#4889=DIRECTION('',(-0.5,0.,-0.866025403784439));
#4890=DIRECTION('center_axis',(-2.40370335797945E-16,0.,1.));
#4891=DIRECTION('ref_axis',(-1.,0.,-2.40370335797945E-16));
#4892=DIRECTION('',(1.,0.,2.40370335797945E-16));
#4893=DIRECTION('',(0.,-1.,0.));
#4894=DIRECTION('',(-1.,0.,-2.40370335797945E-16));
#4895=DIRECTION('center_axis',(0.866025403784439,0.,0.5));
#4896=DIRECTION('ref_axis',(-0.5,0.,0.866025403784439));
#4897=DIRECTION('',(0.5,0.,-0.866025403784439));
#4898=DIRECTION('',(-0.5,0.,0.866025403784439));
#4899=DIRECTION('center_axis',(0.,1.,0.));
#4900=DIRECTION('ref_axis',(1.,0.,0.));
#4901=DIRECTION('center_axis',(0.,-1.,0.));
#4902=DIRECTION('ref_axis',(0.,0.,-1.));
#4903=DIRECTION('center_axis',(0.,1.,0.));
#4904=DIRECTION('ref_axis',(1.,0.,0.));
#4905=DIRECTION('center_axis',(0.,1.,0.));
#4906=DIRECTION('ref_axis',(1.,0.,0.));
#4907=DIRECTION('center_axis',(0.,1.,0.));
#4908=DIRECTION('ref_axis',(0.,0.,1.));
#4909=DIRECTION('center_axis',(0.,-1.,0.));
#4910=DIRECTION('ref_axis',(1.,0.,0.));
#4911=DIRECTION('center_axis',(0.,-1.,0.));
#4912=DIRECTION('ref_axis',(1.,0.,0.));
#4913=DIRECTION('center_axis',(0.,-1.,0.));
#4914=DIRECTION('ref_axis',(1.,0.,0.));
#4915=DIRECTION('',(0.707106781186548,0.707106781186547,8.65956056235493E-17));
#4916=DIRECTION('center_axis',(0.,-1.,0.));
#4917=DIRECTION('ref_axis',(1.,0.,0.));
#4918=DIRECTION('center_axis',(0.,-1.,0.));
#4919=DIRECTION('ref_axis',(1.,0.,0.));
#4920=DIRECTION('',(0.,1.,0.));
#4921=DIRECTION('center_axis',(0.,1.,0.));
#4922=DIRECTION('ref_axis',(1.,0.,0.));
#4923=DIRECTION('center_axis',(0.,-1.,0.));
#4924=DIRECTION('ref_axis',(1.,0.,0.));
#4925=DIRECTION('',(-0.707106781186547,0.707106781186548,-8.65956056235493E-17));
#4926=DIRECTION('center_axis',(0.,-1.,0.));
#4927=DIRECTION('ref_axis',(0.,0.,-1.));
#4928=DIRECTION('center_axis',(0.,-1.,0.));
#4929=DIRECTION('ref_axis',(1.,0.,0.));
#4930=DIRECTION('center_axis',(0.,1.,0.));
#4931=DIRECTION('ref_axis',(1.,0.,0.));
#4932=DIRECTION('center_axis',(0.,1.,0.));
#4933=DIRECTION('ref_axis',(1.,0.,0.));
#4934=DIRECTION('',(-0.447213595499958,0.894427190999916,-5.47678698264203E-17));
#4935=DIRECTION('center_axis',(0.,-1.,0.));
#4936=DIRECTION('ref_axis',(1.,0.,0.));
#4937=DIRECTION('',(0.,1.,0.));
#4938=DIRECTION('axis',(0.,0.,1.));
#4939=DIRECTION('refdir',(1.,0.,0.));
#4940=DIRECTION('axis',(0.,0.,1.));
#4941=DIRECTION('refdir',(1.,0.,0.));
#4942=DIRECTION('center_axis',(0.,1.,0.));
#4943=DIRECTION('ref_axis',(1.,0.,0.));
#4944=DIRECTION('center_axis',(0.,1.,0.));
#4945=DIRECTION('ref_axis',(1.,0.,0.));
#4946=DIRECTION('',(0.,1.,0.));
#4947=DIRECTION('center_axis',(0.,-1.,0.));
#4948=DIRECTION('ref_axis',(1.,0.,0.));
#4949=DIRECTION('center_axis',(0.,1.,0.));
#4950=DIRECTION('ref_axis',(1.,0.,0.));
#4951=DIRECTION('center_axis',(0.,1.,0.));
#4952=DIRECTION('ref_axis',(1.,0.,0.));
#4953=DIRECTION('',(0.,1.,0.));
#4954=DIRECTION('center_axis',(0.,-1.,0.));
#4955=DIRECTION('ref_axis',(1.,0.,0.));
#4956=DIRECTION('center_axis',(0.,1.,0.));
#4957=DIRECTION('ref_axis',(1.,0.,0.));
#4958=DIRECTION('center_axis',(0.,1.,0.));
#4959=DIRECTION('ref_axis',(1.,0.,0.));
#4960=DIRECTION('',(0.,1.,0.));
#4961=DIRECTION('center_axis',(0.,-1.,0.));
#4962=DIRECTION('ref_axis',(1.,0.,0.));
#4963=DIRECTION('center_axis',(0.,1.,0.));
#4964=DIRECTION('ref_axis',(1.,0.,0.));
#4965=DIRECTION('center_axis',(0.,1.,0.));
#4966=DIRECTION('ref_axis',(1.,0.,0.));
#4967=DIRECTION('',(0.,1.,0.));
#4968=DIRECTION('center_axis',(0.,-1.,0.));
#4969=DIRECTION('ref_axis',(1.,0.,0.));
#4970=DIRECTION('center_axis',(0.,1.,0.));
#4971=DIRECTION('ref_axis',(1.,0.,0.));
#4972=DIRECTION('center_axis',(0.,1.,0.));
#4973=DIRECTION('ref_axis',(1.,0.,0.));
#4974=DIRECTION('',(0.,1.,0.));
#4975=DIRECTION('center_axis',(0.,-1.,0.));
#4976=DIRECTION('ref_axis',(1.,0.,0.));
#4977=DIRECTION('center_axis',(0.,1.,0.));
#4978=DIRECTION('ref_axis',(-1.,0.,0.));
#4979=DIRECTION('',(-1.,0.,0.));
#4980=DIRECTION('',(0.,0.,1.));
#4981=DIRECTION('',(-1.,0.,0.));
#4982=DIRECTION('',(0.,0.,1.));
#4983=DIRECTION('center_axis',(1.,0.,0.));
#4984=DIRECTION('ref_axis',(0.,1.,0.));
#4985=DIRECTION('',(0.,1.,0.));
#4986=DIRECTION('',(0.,1.,0.));
#4987=DIRECTION('',(0.,0.,1.));
#4988=DIRECTION('center_axis',(0.,-1.,0.));
#4989=DIRECTION('ref_axis',(1.,0.,0.));
#4990=DIRECTION('',(1.,0.,0.));
#4991=DIRECTION('',(1.,0.,0.));
#4992=DIRECTION('',(0.,0.,1.));
#4993=DIRECTION('center_axis',(-1.,0.,0.));
#4994=DIRECTION('ref_axis',(0.,-1.,0.));
#4995=DIRECTION('',(0.,-1.,0.));
#4996=DIRECTION('',(0.,-1.,0.));
#4997=DIRECTION('center_axis',(0.,0.,1.));
#4998=DIRECTION('ref_axis',(1.,0.,0.));
#4999=DIRECTION('center_axis',(0.,0.,1.));
#5000=DIRECTION('ref_axis',(1.,0.,0.));
#5001=DIRECTION('axis',(0.,0.,1.));
#5002=DIRECTION('refdir',(1.,0.,0.));
#5003=DIRECTION('center_axis',(0.,1.,0.));
#5004=DIRECTION('ref_axis',(1.,0.,0.));
#5005=DIRECTION('center_axis',(0.,1.,0.));
#5006=DIRECTION('ref_axis',(1.,0.,0.));
#5007=DIRECTION('',(0.,1.,0.));
#5008=DIRECTION('center_axis',(0.,-1.,0.));
#5009=DIRECTION('ref_axis',(1.,0.,0.));
#5010=DIRECTION('center_axis',(0.,1.,0.));
#5011=DIRECTION('ref_axis',(1.,0.,0.));
#5012=DIRECTION('center_axis',(0.,1.,0.));
#5013=DIRECTION('ref_axis',(1.,0.,0.));
#5014=DIRECTION('',(0.,1.,0.));
#5015=DIRECTION('center_axis',(0.,-1.,0.));
#5016=DIRECTION('ref_axis',(1.,0.,0.));
#5017=DIRECTION('center_axis',(0.,0.,1.));
#5018=DIRECTION('ref_axis',(1.,0.,0.));
#5019=DIRECTION('center_axis',(0.,0.,1.));
#5020=DIRECTION('ref_axis',(1.,0.,0.));
#5021=DIRECTION('',(0.,0.,1.));
#5022=DIRECTION('center_axis',(0.,0.,-1.));
#5023=DIRECTION('ref_axis',(1.,0.,0.));
#5024=DIRECTION('center_axis',(-1.,0.,0.));
#5025=DIRECTION('ref_axis',(0.,0.,1.));
#5026=DIRECTION('',(0.,1.,0.));
#5027=DIRECTION('',(0.,0.,-1.));
#5028=DIRECTION('',(0.,1.,0.));
#5029=DIRECTION('',(0.,0.,1.));
#5030=DIRECTION('center_axis',(-1.,0.,0.));
#5031=DIRECTION('ref_axis',(0.,0.,1.));
#5032=DIRECTION('',(0.,-1.,0.));
#5033=DIRECTION('',(0.,0.,1.));
#5034=DIRECTION('',(0.,1.,0.));
#5035=DIRECTION('',(0.,0.,-1.));
#5036=DIRECTION('center_axis',(0.,0.,-1.));
#5037=DIRECTION('ref_axis',(-1.,0.,0.));
#5038=DIRECTION('',(1.,0.,0.));
#5039=DIRECTION('',(-1.,0.,0.));
#5040=DIRECTION('',(0.,1.,0.));
#5041=DIRECTION('center_axis',(1.,0.,0.));
#5042=DIRECTION('ref_axis',(0.,0.,-1.));
#5043=DIRECTION('',(0.,0.,1.));
#5044=DIRECTION('',(0.,0.,-1.));
#5045=DIRECTION('',(0.,1.,0.));
#5046=DIRECTION('center_axis',(0.,0.,1.));
#5047=DIRECTION('ref_axis',(1.,0.,0.));
#5048=DIRECTION('',(-1.,0.,0.));
#5049=DIRECTION('',(1.,0.,0.));
#5050=DIRECTION('center_axis',(0.,0.,1.));
#5051=DIRECTION('ref_axis',(1.,0.,0.));
#5052=DIRECTION('',(1.,0.,0.));
#5053=DIRECTION('center_axis',(0.,0.,1.));
#5054=DIRECTION('ref_axis',(1.,0.,0.));
#5055=DIRECTION('',(-1.,0.,0.));
#5056=DIRECTION('center_axis',(0.,1.,0.));
#5057=DIRECTION('ref_axis',(1.,0.,0.));
#5058=DIRECTION('',(-1.,0.,0.));
#5059=DIRECTION('',(0.,0.,1.));
#5060=DIRECTION('center_axis',(0.,1.,0.));
#5061=DIRECTION('ref_axis',(0.,0.,1.));
#5062=DIRECTION('',(0.,0.,-1.));
#5063=DIRECTION('',(1.,0.,0.));
#5064=DIRECTION('center_axis',(0.,0.,1.));
#5065=DIRECTION('ref_axis',(-0.934172358962716,0.35682208977309,0.));
#5066=DIRECTION('center_axis',(0.,0.,1.));
#5067=DIRECTION('ref_axis',(1.,0.,0.));
#5068=DIRECTION('center_axis',(0.,0.,1.));
#5069=DIRECTION('ref_axis',(1.,0.,0.));
#5070=DIRECTION('axis',(0.,0.,1.));
#5071=DIRECTION('refdir',(1.,0.,0.));
#5072=DIRECTION('center_axis',(0.,1.,0.));
#5073=DIRECTION('ref_axis',(0.,0.,1.));
#5074=DIRECTION('center_axis',(0.,-1.,0.));
#5075=DIRECTION('ref_axis',(1.,0.,0.));
#5076=DIRECTION('center_axis',(0.,-1.,0.));
#5077=DIRECTION('ref_axis',(1.,0.,0.));
#5078=DIRECTION('center_axis',(0.,-1.,0.));
#5079=DIRECTION('ref_axis',(1.,0.,0.));
#5080=DIRECTION('',(0.707106781186547,0.707106781186548,8.65956056235493E-17));
#5081=DIRECTION('center_axis',(0.,-1.,0.));
#5082=DIRECTION('ref_axis',(1.,0.,0.));
#5083=DIRECTION('center_axis',(0.,-1.,0.));
#5084=DIRECTION('ref_axis',(1.,0.,0.));
#5085=DIRECTION('',(0.,1.,0.));
#5086=DIRECTION('center_axis',(0.,1.,0.));
#5087=DIRECTION('ref_axis',(1.,0.,0.));
#5088=DIRECTION('center_axis',(0.,-1.,0.));
#5089=DIRECTION('ref_axis',(1.,0.,0.));
#5090=DIRECTION('',(-0.707106781186547,0.707106781186548,-8.65956056235493E-17));
#5091=DIRECTION('center_axis',(0.,-1.,0.));
#5092=DIRECTION('ref_axis',(0.,0.,-1.));
#5093=DIRECTION('center_axis',(0.,-1.,0.));
#5094=DIRECTION('ref_axis',(1.,0.,0.));
#5095=DIRECTION('center_axis',(0.,1.,0.));
#5096=DIRECTION('ref_axis',(1.,0.,0.));
#5097=DIRECTION('center_axis',(0.,1.,0.));
#5098=DIRECTION('ref_axis',(1.,0.,0.));
#5099=DIRECTION('',(-0.447213595499958,0.894427190999916,-5.47678698264203E-17));
#5100=DIRECTION('center_axis',(0.,-1.,0.));
#5101=DIRECTION('ref_axis',(1.,0.,0.));
#5102=DIRECTION('center_axis',(0.,1.,0.));
#5103=DIRECTION('ref_axis',(1.,0.,0.));
#5104=DIRECTION('',(0.,1.,0.));
#5105=DIRECTION('center_axis',(0.,1.,0.));
#5106=DIRECTION('ref_axis',(1.,0.,0.));
#5107=DIRECTION('center_axis',(0.,-1.,0.));
#5108=DIRECTION('ref_axis',(1.,0.,0.));
#5109=DIRECTION('',(-0.707106781186547,0.707106781186548,-8.65956056235493E-17));
#5110=DIRECTION('center_axis',(0.,-1.,0.));
#5111=DIRECTION('ref_axis',(0.,0.,-1.));
#5112=DIRECTION('center_axis',(0.866025403784439,0.,-0.5));
#5113=DIRECTION('ref_axis',(0.5,0.,0.866025403784439));
#5114=DIRECTION('',(-0.5,0.,-0.866025403784439));
#5115=DIRECTION('',(0.,-1.,0.));
#5116=DIRECTION('',(0.5,0.,0.866025403784439));
#5117=DIRECTION('',(0.,-1.,0.));
#5118=DIRECTION('center_axis',(1.60246890531964E-16,0.,-1.));
#5119=DIRECTION('ref_axis',(1.,0.,1.60246890531964E-16));
#5120=DIRECTION('',(-1.,0.,-1.60246890531964E-16));
#5121=DIRECTION('',(0.,-1.,0.));
#5122=DIRECTION('',(1.,0.,1.60246890531964E-16));
#5123=DIRECTION('center_axis',(-0.866025403784439,0.,-0.5));
#5124=DIRECTION('ref_axis',(0.5,0.,-0.866025403784439));
#5125=DIRECTION('',(-0.5,0.,0.866025403784439));
#5126=DIRECTION('',(0.,-1.,0.));
#5127=DIRECTION('',(0.5,0.,-0.866025403784439));
#5128=DIRECTION('center_axis',(-0.866025403784439,0.,0.5));
#5129=DIRECTION('ref_axis',(-0.5,0.,-0.866025403784439));
#5130=DIRECTION('',(0.5,0.,0.866025403784439));
#5131=DIRECTION('',(0.,-1.,0.));
#5132=DIRECTION('',(-0.5,0.,-0.866025403784439));
#5133=DIRECTION('center_axis',(-1.60246890531964E-16,0.,1.));
#5134=DIRECTION('ref_axis',(-1.,0.,-1.60246890531964E-16));
#5135=DIRECTION('',(1.,0.,1.60246890531964E-16));
#5136=DIRECTION('',(0.,-1.,0.));
#5137=DIRECTION('',(-1.,0.,-1.60246890531964E-16));
#5138=DIRECTION('center_axis',(0.866025403784439,0.,0.5));
#5139=DIRECTION('ref_axis',(-0.5,0.,0.866025403784439));
#5140=DIRECTION('',(0.5,0.,-0.866025403784439));
#5141=DIRECTION('',(-0.5,0.,0.866025403784439));
#5142=DIRECTION('center_axis',(0.,1.,0.));
#5143=DIRECTION('ref_axis',(1.,0.,0.));
#5144=DIRECTION('center_axis',(0.,-1.,0.));
#5145=DIRECTION('ref_axis',(0.,0.,-1.));
#5146=DIRECTION('axis',(0.,0.,1.));
#5147=DIRECTION('refdir',(1.,0.,0.));
#5148=DIRECTION('center_axis',(0.,1.,0.));
#5149=DIRECTION('ref_axis',(1.,0.,0.));
#5150=DIRECTION('',(0.866025403784439,-0.5,1.06057523872491E-16));
#5151=DIRECTION('center_axis',(0.,-1.,0.));
#5152=DIRECTION('ref_axis',(1.,0.,0.));
#5153=DIRECTION('center_axis',(0.,-1.,0.));
#5154=DIRECTION('ref_axis',(1.,0.,0.));
#5155=DIRECTION('center_axis',(0.,1.,0.));
#5156=DIRECTION('ref_axis',(1.,0.,0.));
#5157=DIRECTION('',(-0.866025403784439,-0.5,-1.06057523872491E-16));
#5158=DIRECTION('center_axis',(1.37354477598826E-16,0.,-1.));
#5159=DIRECTION('ref_axis',(-1.,0.,-1.37354477598826E-16));
#5160=DIRECTION('',(0.,1.,0.));
#5161=DIRECTION('',(0.,1.,0.));
#5162=DIRECTION('center_axis',(-0.866025403784439,0.,-0.5));
#5163=DIRECTION('ref_axis',(-0.5,0.,0.866025403784439));
#5164=DIRECTION('',(0.,1.,0.));
#5165=DIRECTION('center_axis',(-0.866025403784439,0.,0.5));
#5166=DIRECTION('ref_axis',(0.5,0.,0.866025403784439));
#5167=DIRECTION('',(0.,1.,0.));
#5168=DIRECTION('center_axis',(0.,1.,0.));
#5169=DIRECTION('ref_axis',(1.,0.,0.));
#5170=DIRECTION('center_axis',(0.,1.,0.));
#5171=DIRECTION('ref_axis',(1.,0.,0.));
#5172=DIRECTION('',(0.,-1.,0.));
#5173=DIRECTION('center_axis',(0.,1.,0.));
#5174=DIRECTION('ref_axis',(1.,0.,0.));
#5175=DIRECTION('center_axis',(-1.37354477598826E-16,0.,1.));
#5176=DIRECTION('ref_axis',(1.,0.,1.37354477598826E-16));
#5177=DIRECTION('',(0.,1.,0.));
#5178=DIRECTION('center_axis',(0.866025403784439,0.,-0.5));
#5179=DIRECTION('ref_axis',(-0.5,0.,-0.866025403784439));
#5180=DIRECTION('',(0.,1.,0.));
#5181=DIRECTION('center_axis',(0.866025403784439,0.,0.5));
#5182=DIRECTION('ref_axis',(0.5,0.,-0.866025403784439));
#5183=DIRECTION('center_axis',(0.,1.,0.));
#5184=DIRECTION('ref_axis',(1.,0.,0.));
#5185=DIRECTION('center_axis',(0.,1.,0.));
#5186=DIRECTION('ref_axis',(1.,0.,0.));
#5187=DIRECTION('axis',(0.,0.,1.));
#5188=DIRECTION('refdir',(1.,0.,0.));
#5189=DIRECTION('center_axis',(0.,1.,0.));
#5190=DIRECTION('ref_axis',(1.,0.,0.));
#5191=DIRECTION('center_axis',(0.,1.,0.));
#5192=DIRECTION('ref_axis',(1.,0.,0.));
#5193=DIRECTION('',(0.707106781186548,-0.707106781186547,-8.65956056235494E-17));
#5194=DIRECTION('center_axis',(0.,-1.,0.));
#5195=DIRECTION('ref_axis',(1.,0.,0.));
#5196=DIRECTION('center_axis',(0.,1.,0.));
#5197=DIRECTION('ref_axis',(1.,0.,0.));
#5198=DIRECTION('',(0.,-1.,0.));
#5199=DIRECTION('center_axis',(0.,-1.,0.));
#5200=DIRECTION('ref_axis',(1.,0.,0.));
#5201=DIRECTION('center_axis',(0.,1.,0.));
#5202=DIRECTION('ref_axis',(1.,0.,0.));
#5203=DIRECTION('center_axis',(0.,1.,0.));
#5204=DIRECTION('ref_axis',(1.,0.,0.));
#5205=DIRECTION('center_axis',(0.,1.,0.));
#5206=DIRECTION('ref_axis',(1.,0.,0.));
#5207=DIRECTION('',(0.,-1.,0.));
#5208=DIRECTION('center_axis',(0.,1.,0.));
#5209=DIRECTION('ref_axis',(1.,0.,0.));
#5210=DIRECTION('center_axis',(0.,1.,0.));
#5211=DIRECTION('ref_axis',(1.,0.,0.));
#5212=DIRECTION('',(0.,0.,1.));
#5213=DIRECTION('',(1.,0.,0.));
#5214=DIRECTION('',(0.,0.,1.));
#5215=DIRECTION('',(1.,0.,0.));
#5216=DIRECTION('',(-1.,0.,2.22044604925031E-16));
#5217=DIRECTION('',(2.22044604925031E-16,0.,1.));
#5218=DIRECTION('',(-1.,0.,2.22044604925031E-16));
#5219=DIRECTION('',(2.22044604925031E-16,0.,1.));
#5220=DIRECTION('',(0.,0.,1.));
#5221=DIRECTION('',(1.,0.,0.));
#5222=DIRECTION('',(0.,-1.,2.22044604925031E-16));
#5223=DIRECTION('',(1.,0.,0.));
#5224=DIRECTION('',(0.,-1.,2.22044604925031E-16));
#5225=DIRECTION('',(1.,0.,0.));
#5226=DIRECTION('',(0.,-1.,2.22044604925031E-16));
#5227=DIRECTION('',(1.,0.,0.));
#5228=DIRECTION('',(1.11022302462516E-16,1.,0.));
#5229=DIRECTION('',(0.,1.11022302462516E-16,-1.));
#5230=DIRECTION('',(-1.11022302462516E-16,-1.,0.));
#5231=DIRECTION('',(0.,1.11022302462516E-16,1.));
#5232=DIRECTION('',(0.,0.,1.));
#5233=DIRECTION('',(-1.,1.22464679914735E-16,0.));
#5234=DIRECTION('',(0.,0.,1.));
#5235=DIRECTION('',(-1.,1.22464679914735E-16,0.));
#5236=DIRECTION('',(-1.11022302462516E-16,-1.,0.));
#5237=DIRECTION('',(0.,1.11022302462516E-16,1.));
#5238=DIRECTION('',(0.,0.,1.));
#5239=DIRECTION('',(-1.,1.22464679914735E-16,0.));
#5240=DIRECTION('',(0.,0.,1.));
#5241=DIRECTION('',(-1.,1.22464679914735E-16,0.));
#5242=DIRECTION('',(0.,-1.,2.22044604925031E-16));
#5243=DIRECTION('',(1.,0.,0.));
#5244=DIRECTION('',(0.,-1.,2.22044604925031E-16));
#5245=DIRECTION('',(1.,0.,0.));
#5246=DIRECTION('',(0.,-1.,2.22044604925031E-16));
#5247=DIRECTION('',(1.,0.,0.));
#5248=DIRECTION('',(1.11022302462516E-16,1.,0.));
#5249=DIRECTION('',(0.,1.11022302462516E-16,-1.));
#5250=DIRECTION('',(-1.11022302462516E-16,-1.,0.));
#5251=DIRECTION('',(0.,1.11022302462516E-16,1.));
#5252=DIRECTION('',(0.,0.,1.));
#5253=DIRECTION('',(-1.,1.22464679914735E-16,0.));
#5254=DIRECTION('',(0.,0.,1.));
#5255=DIRECTION('',(-1.,1.22464679914735E-16,0.));
#5256=DIRECTION('',(-1.11022302462516E-16,-1.,0.));
#5257=DIRECTION('',(0.,1.11022302462516E-16,1.));
#5258=DIRECTION('',(0.,0.,1.));
#5259=DIRECTION('',(-1.,1.22464679914735E-16,0.));
#5260=DIRECTION('',(0.,0.,1.));
#5261=DIRECTION('',(-1.,1.22464679914735E-16,0.));
#5262=DIRECTION('',(-1.11022302462516E-16,-1.,0.));
#5263=DIRECTION('',(0.,1.11022302462516E-16,1.));
#5264=DIRECTION('',(0.,0.,1.));
#5265=DIRECTION('',(-1.,1.22464679914735E-16,0.));
#5266=DIRECTION('',(0.,0.,1.));
#5267=DIRECTION('',(-1.,1.22464679914735E-16,0.));
#5268=DIRECTION('',(-1.11022302462516E-16,-1.,0.));
#5269=DIRECTION('',(0.,1.11022302462516E-16,1.));
#5270=DIRECTION('',(0.,0.,1.));
#5271=DIRECTION('',(-1.,1.22464679914735E-16,0.));
#5272=DIRECTION('',(0.,0.,1.));
#5273=DIRECTION('',(-1.,1.22464679914735E-16,0.));
#5274=DIRECTION('axis',(0.,0.,1.));
#5275=DIRECTION('refdir',(1.,0.,0.));
#5276=DIRECTION('center_axis',(0.,1.,0.));
#5277=DIRECTION('ref_axis',(0.,0.,1.));
#5278=DIRECTION('center_axis',(0.,-1.,0.));
#5279=DIRECTION('ref_axis',(1.,0.,0.));
#5280=DIRECTION('center_axis',(0.,-1.,0.));
#5281=DIRECTION('ref_axis',(1.,0.,0.));
#5282=DIRECTION('center_axis',(0.,-1.,0.));
#5283=DIRECTION('ref_axis',(1.,0.,0.));
#5284=DIRECTION('',(0.707106781186548,0.707106781186547,8.65956056235493E-17));
#5285=DIRECTION('center_axis',(0.,-1.,0.));
#5286=DIRECTION('ref_axis',(1.,0.,0.));
#5287=DIRECTION('center_axis',(0.,-1.,0.));
#5288=DIRECTION('ref_axis',(1.,0.,0.));
#5289=DIRECTION('',(0.,1.,0.));
#5290=DIRECTION('center_axis',(0.,1.,0.));
#5291=DIRECTION('ref_axis',(1.,0.,0.));
#5292=DIRECTION('center_axis',(0.,-1.,0.));
#5293=DIRECTION('ref_axis',(1.,0.,0.));
#5294=DIRECTION('',(-0.707106781186547,0.707106781186548,-8.65956056235493E-17));
#5295=DIRECTION('center_axis',(0.,-1.,0.));
#5296=DIRECTION('ref_axis',(0.,0.,-1.));
#5297=DIRECTION('center_axis',(0.,-1.,0.));
#5298=DIRECTION('ref_axis',(1.,0.,0.));
#5299=DIRECTION('center_axis',(0.,1.,0.));
#5300=DIRECTION('ref_axis',(1.,0.,0.));
#5301=DIRECTION('center_axis',(0.,1.,0.));
#5302=DIRECTION('ref_axis',(1.,0.,0.));
#5303=DIRECTION('',(-0.447213595499958,0.894427190999916,-5.47678698264203E-17));
#5304=DIRECTION('center_axis',(0.,-1.,0.));
#5305=DIRECTION('ref_axis',(1.,0.,0.));
#5306=DIRECTION('center_axis',(0.,1.,0.));
#5307=DIRECTION('ref_axis',(1.,0.,0.));
#5308=DIRECTION('',(0.,1.,0.));
#5309=DIRECTION('center_axis',(0.,1.,0.));
#5310=DIRECTION('ref_axis',(1.,0.,0.));
#5311=DIRECTION('center_axis',(0.,-1.,0.));
#5312=DIRECTION('ref_axis',(1.,0.,0.));
#5313=DIRECTION('',(-0.707106781186547,0.707106781186548,-8.65956056235493E-17));
#5314=DIRECTION('center_axis',(0.,-1.,0.));
#5315=DIRECTION('ref_axis',(0.,0.,-1.));
#5316=DIRECTION('center_axis',(0.866025403784439,0.,-0.5));
#5317=DIRECTION('ref_axis',(0.5,0.,0.866025403784439));
#5318=DIRECTION('',(-0.5,0.,-0.866025403784439));
#5319=DIRECTION('',(0.,-1.,0.));
#5320=DIRECTION('',(0.5,0.,0.866025403784439));
#5321=DIRECTION('',(0.,-1.,0.));
#5322=DIRECTION('center_axis',(1.20185167898973E-16,0.,-1.));
#5323=DIRECTION('ref_axis',(1.,0.,1.20185167898973E-16));
#5324=DIRECTION('',(-1.,0.,-1.20185167898973E-16));
#5325=DIRECTION('',(0.,-1.,0.));
#5326=DIRECTION('',(1.,0.,1.20185167898973E-16));
#5327=DIRECTION('center_axis',(-0.866025403784439,0.,-0.5));
#5328=DIRECTION('ref_axis',(0.5,0.,-0.866025403784439));
#5329=DIRECTION('',(-0.5,0.,0.866025403784439));
#5330=DIRECTION('',(0.,-1.,0.));
#5331=DIRECTION('',(0.5,0.,-0.866025403784439));
#5332=DIRECTION('center_axis',(-0.866025403784439,0.,0.5));
#5333=DIRECTION('ref_axis',(-0.5,0.,-0.866025403784439));
#5334=DIRECTION('',(0.5,0.,0.866025403784439));
#5335=DIRECTION('',(0.,-1.,0.));
#5336=DIRECTION('',(-0.5,0.,-0.866025403784439));
#5337=DIRECTION('center_axis',(-2.40370335797945E-16,0.,1.));
#5338=DIRECTION('ref_axis',(-1.,0.,-2.40370335797945E-16));
#5339=DIRECTION('',(1.,0.,2.40370335797945E-16));
#5340=DIRECTION('',(0.,-1.,0.));
#5341=DIRECTION('',(-1.,0.,-2.40370335797945E-16));
#5342=DIRECTION('center_axis',(0.866025403784439,0.,0.5));
#5343=DIRECTION('ref_axis',(-0.5,0.,0.866025403784439));
#5344=DIRECTION('',(0.5,0.,-0.866025403784439));
#5345=DIRECTION('',(-0.5,0.,0.866025403784439));
#5346=DIRECTION('center_axis',(0.,1.,0.));
#5347=DIRECTION('ref_axis',(1.,0.,0.));
#5348=DIRECTION('center_axis',(0.,-1.,0.));
#5349=DIRECTION('ref_axis',(0.,0.,-1.));
#5350=DIRECTION('axis',(0.,0.,1.));
#5351=DIRECTION('refdir',(1.,0.,0.));
#5352=DIRECTION('center_axis',(0.,1.,0.));
#5353=DIRECTION('ref_axis',(1.,0.,0.));
#5354=DIRECTION('',(0.866025403784439,-0.5,1.06057523872491E-16));
#5355=DIRECTION('center_axis',(0.,-1.,0.));
#5356=DIRECTION('ref_axis',(1.,0.,0.));
#5357=DIRECTION('center_axis',(0.,-1.,0.));
#5358=DIRECTION('ref_axis',(1.,0.,0.));
#5359=DIRECTION('center_axis',(0.,1.,0.));
#5360=DIRECTION('ref_axis',(1.,0.,0.));
#5361=DIRECTION('',(-0.866025403784439,-0.5,-1.06057523872491E-16));
#5362=DIRECTION('center_axis',(1.20185167898973E-16,0.,-1.));
#5363=DIRECTION('ref_axis',(-1.,0.,-1.20185167898973E-16));
#5364=DIRECTION('',(0.,1.,0.));
#5365=DIRECTION('',(0.,1.,0.));
#5366=DIRECTION('center_axis',(-0.866025403784439,0.,-0.5));
#5367=DIRECTION('ref_axis',(-0.5,0.,0.866025403784439));
#5368=DIRECTION('',(0.,1.,0.));
#5369=DIRECTION('center_axis',(-0.866025403784439,0.,0.5));
#5370=DIRECTION('ref_axis',(0.5,0.,0.866025403784439));
#5371=DIRECTION('',(0.,1.,0.));
#5372=DIRECTION('center_axis',(0.,1.,0.));
#5373=DIRECTION('ref_axis',(1.,0.,0.));
#5374=DIRECTION('center_axis',(0.,1.,0.));
#5375=DIRECTION('ref_axis',(1.,0.,0.));
#5376=DIRECTION('',(0.,-1.,0.));
#5377=DIRECTION('center_axis',(0.,1.,0.));
#5378=DIRECTION('ref_axis',(1.,0.,0.));
#5379=DIRECTION('center_axis',(-2.40370335797945E-16,0.,1.));
#5380=DIRECTION('ref_axis',(1.,0.,2.40370335797945E-16));
#5381=DIRECTION('',(0.,1.,0.));
#5382=DIRECTION('center_axis',(0.866025403784439,0.,-0.5));
#5383=DIRECTION('ref_axis',(-0.5,0.,-0.866025403784439));
#5384=DIRECTION('',(0.,1.,0.));
#5385=DIRECTION('center_axis',(0.866025403784439,0.,0.5));
#5386=DIRECTION('ref_axis',(0.5,0.,-0.866025403784439));
#5387=DIRECTION('center_axis',(0.,1.,0.));
#5388=DIRECTION('ref_axis',(1.,0.,0.));
#5389=DIRECTION('center_axis',(0.,1.,0.));
#5390=DIRECTION('ref_axis',(1.,0.,0.));
#5391=DIRECTION('',(0.,0.,1.));
#5392=DIRECTION('',(1.,0.,0.));
#5393=DIRECTION('',(0.,0.,1.));
#5394=DIRECTION('',(1.,0.,0.));
#5395=DIRECTION('',(0.,0.,1.));
#5396=DIRECTION('',(1.,0.,0.));
#5397=DIRECTION('',(0.,0.,1.));
#5398=DIRECTION('',(-1.,1.22464679914735E-16,0.));
#5399=DIRECTION('',(0.,0.,1.));
#5400=DIRECTION('',(1.,0.,0.));
#5401=DIRECTION('',(0.,0.,1.));
#5402=DIRECTION('',(-1.,1.22464679914735E-16,0.));
#5403=DIRECTION('',(0.,0.,1.));
#5404=DIRECTION('',(1.,0.,0.));
#5405=DIRECTION('',(0.,0.,1.));
#5406=DIRECTION('',(-1.,1.22464679914735E-16,0.));
#5407=DIRECTION('',(0.,0.,1.));
#5408=DIRECTION('',(1.,0.,0.));
#5409=DIRECTION('',(0.,0.,1.));
#5410=DIRECTION('',(-1.,1.22464679914735E-16,0.));
#5411=DIRECTION('',(0.,0.,1.));
#5412=DIRECTION('',(1.,0.,0.));
#5413=DIRECTION('',(0.,0.,1.));
#5414=DIRECTION('',(-1.,1.22464679914735E-16,0.));
#5415=DIRECTION('',(0.,0.,1.));
#5416=DIRECTION('',(-1.,1.22464679914735E-16,0.));
#5417=DIRECTION('',(0.,0.,1.));
#5418=DIRECTION('',(1.,0.,0.));
#5419=DIRECTION('axis',(0.,0.,1.));
#5420=DIRECTION('refdir',(1.,0.,0.));
#5421=DIRECTION('axis',(0.,0.,1.));
#5422=DIRECTION('refdir',(1.,0.,0.));
#5423=DIRECTION('center_axis',(0.,1.,0.));
#5424=DIRECTION('ref_axis',(1.,0.,0.));
#5425=DIRECTION('center_axis',(0.,1.,0.));
#5426=DIRECTION('ref_axis',(1.,0.,0.));
#5427=DIRECTION('',(0.,1.,0.));
#5428=DIRECTION('center_axis',(0.,-1.,0.));
#5429=DIRECTION('ref_axis',(1.,0.,0.));
#5430=DIRECTION('center_axis',(0.,1.,0.));
#5431=DIRECTION('ref_axis',(-1.,0.,0.));
#5432=DIRECTION('',(-1.,0.,0.));
#5433=DIRECTION('',(0.,0.,1.));
#5434=DIRECTION('',(-1.,0.,0.));
#5435=DIRECTION('',(0.,0.,1.));
#5436=DIRECTION('center_axis',(1.,0.,0.));
#5437=DIRECTION('ref_axis',(0.,1.,0.));
#5438=DIRECTION('',(0.,1.,0.));
#5439=DIRECTION('',(0.,1.,0.));
#5440=DIRECTION('',(0.,0.,1.));
#5441=DIRECTION('center_axis',(0.,-1.,0.));
#5442=DIRECTION('ref_axis',(1.,0.,0.));
#5443=DIRECTION('',(1.,0.,0.));
#5444=DIRECTION('',(1.,0.,0.));
#5445=DIRECTION('',(0.,0.,1.));
#5446=DIRECTION('center_axis',(-1.,0.,0.));
#5447=DIRECTION('ref_axis',(0.,-1.,0.));
#5448=DIRECTION('',(0.,-1.,0.));
#5449=DIRECTION('',(0.,-1.,0.));
#5450=DIRECTION('center_axis',(0.,0.,1.));
#5451=DIRECTION('ref_axis',(1.,0.,0.));
#5452=DIRECTION('center_axis',(0.,0.,1.));
#5453=DIRECTION('ref_axis',(1.,0.,0.));
#5454=DIRECTION('',(0.,0.,1.));
#5455=DIRECTION('',(1.,0.,0.));
#5456=DIRECTION('',(0.,0.,1.));
#5457=DIRECTION('',(1.,0.,0.));
#5458=DIRECTION('',(0.,0.,1.));
#5459=DIRECTION('',(1.,0.,0.));
#5460=DIRECTION('',(0.,0.,1.));
#5461=DIRECTION('',(1.,0.,0.));
#5462=CARTESIAN_POINT('',(0.,0.,0.));
#5463=CARTESIAN_POINT('',(0.,0.,0.));
#5464=CARTESIAN_POINT('',(0.,0.,0.));
#5465=CARTESIAN_POINT('Origin',(22.,-1.9,15.));
#5466=CARTESIAN_POINT('',(21.725,-1.8,15.));
#5467=CARTESIAN_POINT('Origin',(22.,-1.8,15.));
#5468=CARTESIAN_POINT('',(21.725,-1.,15.));
#5469=CARTESIAN_POINT('',(21.725,-1.9,15.));
#5470=CARTESIAN_POINT('Origin',(22.,-1.,15.));
#5471=CARTESIAN_POINT('Origin',(22.,-1.9,17.));
#5472=CARTESIAN_POINT('',(21.725,-1.8,17.));
#5473=CARTESIAN_POINT('Origin',(22.,-1.8,17.));
#5474=CARTESIAN_POINT('',(21.725,-1.,17.));
#5475=CARTESIAN_POINT('',(21.725,-1.9,17.));
#5476=CARTESIAN_POINT('Origin',(22.,-1.,17.));
#5477=CARTESIAN_POINT('Origin',(23.,-1.,14.5));
#5478=CARTESIAN_POINT('',(23.,-1.,14.5));
#5479=CARTESIAN_POINT('',(21.,-1.,14.5));
#5480=CARTESIAN_POINT('',(23.,-1.,14.5));
#5481=CARTESIAN_POINT('',(21.,-1.,17.5));
#5482=CARTESIAN_POINT('',(21.,-1.,14.5));
#5483=CARTESIAN_POINT('',(23.,-1.,17.5));
#5484=CARTESIAN_POINT('',(23.,-1.,17.5));
#5485=CARTESIAN_POINT('',(23.,-1.,14.5));
#5486=CARTESIAN_POINT('Origin',(23.,-1.8,14.5));
#5487=CARTESIAN_POINT('',(23.,-1.8,14.5));
#5488=CARTESIAN_POINT('',(23.,-1.8,14.5));
#5489=CARTESIAN_POINT('',(23.,-1.8,17.5));
#5490=CARTESIAN_POINT('',(23.,-1.8,17.5));
#5491=CARTESIAN_POINT('',(23.,-1.8,14.5));
#5492=CARTESIAN_POINT('Origin',(21.,-1.8,14.5));
#5493=CARTESIAN_POINT('',(21.,-1.8,14.5));
#5494=CARTESIAN_POINT('',(21.,-1.8,14.5));
#5495=CARTESIAN_POINT('',(21.,-1.8,17.5));
#5496=CARTESIAN_POINT('',(21.,-1.8,17.5));
#5497=CARTESIAN_POINT('',(21.,-1.8,14.5));
#5498=CARTESIAN_POINT('Origin',(21.,-1.,14.5));
#5499=CARTESIAN_POINT('',(21.,-1.,14.5));
#5500=CARTESIAN_POINT('',(21.,-1.,17.5));
#5501=CARTESIAN_POINT('Origin',(22.,-1.4,17.5));
#5502=CARTESIAN_POINT('Origin',(22.,-1.4,14.5));
#5503=CARTESIAN_POINT('',(0.,0.,0.));
#5504=CARTESIAN_POINT('Origin',(-0.1,0.82,-0.3));
#5505=CARTESIAN_POINT('',(0.,0.82,-0.3));
#5506=CARTESIAN_POINT('',(0.,1.,-0.3));
#5507=CARTESIAN_POINT('',(0.,0.41,-0.3));
#5508=CARTESIAN_POINT('',(30.,0.82,-0.3));
#5509=CARTESIAN_POINT('',(-0.1,0.82,-0.3));
#5510=CARTESIAN_POINT('',(30.,1.,-0.3));
#5511=CARTESIAN_POINT('',(30.,0.41,-0.3));
#5512=CARTESIAN_POINT('',(-0.05,1.,-0.3));
#5513=CARTESIAN_POINT('Origin',(-0.1,0.82,-0.55));
#5514=CARTESIAN_POINT('',(0.,0.82,-0.55));
#5515=CARTESIAN_POINT('',(0.,0.82,-0.275));
#5516=CARTESIAN_POINT('',(30.,0.82,-0.55));
#5517=CARTESIAN_POINT('',(-0.1,0.82,-0.55));
#5518=CARTESIAN_POINT('',(30.,0.82,-0.275));
#5519=CARTESIAN_POINT('Origin',(-0.1,0.67,-0.55));
#5520=CARTESIAN_POINT('',(0.,0.67,-0.55));
#5521=CARTESIAN_POINT('',(0.,0.335,-0.55));
#5522=CARTESIAN_POINT('',(30.,0.67,-0.55));
#5523=CARTESIAN_POINT('',(-0.1,0.67,-0.55));
#5524=CARTESIAN_POINT('',(30.,0.335,-0.55));
#5525=CARTESIAN_POINT('Origin',(-0.1,0.42,-0.3));
#5526=CARTESIAN_POINT('',(0.,0.42,-0.3));
#5527=CARTESIAN_POINT('',(0.,0.24,-0.12));
#5528=CARTESIAN_POINT('',(30.,0.42,-0.3));
#5529=CARTESIAN_POINT('',(-0.1,0.42,-0.3));
#5530=CARTESIAN_POINT('',(30.,0.24,-0.12));
#5531=CARTESIAN_POINT('Origin',(-0.1,0.42,0.3));
#5532=CARTESIAN_POINT('',(0.,0.42,0.3));
#5533=CARTESIAN_POINT('',(0.,0.42,0.15));
#5534=CARTESIAN_POINT('',(30.,0.42,0.3));
#5535=CARTESIAN_POINT('',(-0.1,0.42,0.3));
#5536=CARTESIAN_POINT('',(30.,0.42,0.15));
#5537=CARTESIAN_POINT('Origin',(-0.1,0.67,0.55));
#5538=CARTESIAN_POINT('',(0.,0.67,0.55));
#5539=CARTESIAN_POINT('',(6.93889390390723E-18,0.365,0.245));
#5540=CARTESIAN_POINT('',(30.,0.67,0.55));
#5541=CARTESIAN_POINT('',(-0.1,0.67,0.55));
#5542=CARTESIAN_POINT('',(30.,0.365,0.245));
#5543=CARTESIAN_POINT('Origin',(-0.1,0.82,0.55));
#5544=CARTESIAN_POINT('',(0.,0.82,0.55));
#5545=CARTESIAN_POINT('',(0.,0.41,0.55));
#5546=CARTESIAN_POINT('',(30.,0.82,0.55));
#5547=CARTESIAN_POINT('',(-0.1,0.82,0.55));
#5548=CARTESIAN_POINT('',(30.,0.41,0.55));
#5549=CARTESIAN_POINT('Origin',(-0.1,0.82,0.3));
#5550=CARTESIAN_POINT('',(0.,0.82,0.3));
#5551=CARTESIAN_POINT('',(0.,0.82,0.15));
#5552=CARTESIAN_POINT('',(30.,0.82,0.3));
#5553=CARTESIAN_POINT('',(-0.1,0.82,0.3));
#5554=CARTESIAN_POINT('',(30.,0.82,0.15));
#5555=CARTESIAN_POINT('Origin',(-0.1,1.05,0.3));
#5556=CARTESIAN_POINT('',(0.,1.,0.3));
#5557=CARTESIAN_POINT('',(0.,0.525,0.3));
#5558=CARTESIAN_POINT('',(30.,1.,0.3));
#5559=CARTESIAN_POINT('',(-0.05,1.,0.3));
#5560=CARTESIAN_POINT('',(30.,0.525,0.3));
#5561=CARTESIAN_POINT('Origin',(-0.1,-0.3,-0.82));
#5562=CARTESIAN_POINT('',(0.,-0.3,-0.82));
#5563=CARTESIAN_POINT('',(0.,-0.3,-1.));
#5564=CARTESIAN_POINT('',(0.,-0.3,-0.41));
#5565=CARTESIAN_POINT('',(30.,-0.3,-0.82));
#5566=CARTESIAN_POINT('',(-0.1,-0.3,-0.82));
#5567=CARTESIAN_POINT('',(30.,-0.3,-1.));
#5568=CARTESIAN_POINT('',(30.,-0.3,-0.41));
#5569=CARTESIAN_POINT('',(-0.05,-0.3,-1.));
#5570=CARTESIAN_POINT('Origin',(-0.1,-0.55,-0.82));
#5571=CARTESIAN_POINT('',(0.,-0.55,-0.82));
#5572=CARTESIAN_POINT('',(0.,-0.275,-0.82));
#5573=CARTESIAN_POINT('',(30.,-0.55,-0.82));
#5574=CARTESIAN_POINT('',(-0.1,-0.55,-0.82));
#5575=CARTESIAN_POINT('',(30.,-0.275,-0.82));
#5576=CARTESIAN_POINT('Origin',(-0.1,-0.55,-0.67));
#5577=CARTESIAN_POINT('',(0.,-0.55,-0.67));
#5578=CARTESIAN_POINT('',(0.,-0.55,-0.335));
#5579=CARTESIAN_POINT('',(30.,-0.55,-0.67));
#5580=CARTESIAN_POINT('',(-0.1,-0.55,-0.67));
#5581=CARTESIAN_POINT('',(30.,-0.55,-0.335));
#5582=CARTESIAN_POINT('Origin',(-0.1,-0.3,-0.42));
#5583=CARTESIAN_POINT('',(0.,-0.3,-0.42));
#5584=CARTESIAN_POINT('',(0.,-0.12,-0.24));
#5585=CARTESIAN_POINT('',(30.,-0.3,-0.42));
#5586=CARTESIAN_POINT('',(-0.1,-0.3,-0.42));
#5587=CARTESIAN_POINT('',(30.,-0.12,-0.24));
#5588=CARTESIAN_POINT('Origin',(-0.1,0.3,-0.42));
#5589=CARTESIAN_POINT('',(0.,0.3,-0.42));
#5590=CARTESIAN_POINT('',(0.,0.15,-0.42));
#5591=CARTESIAN_POINT('',(30.,0.3,-0.42));
#5592=CARTESIAN_POINT('',(-0.1,0.3,-0.42));
#5593=CARTESIAN_POINT('',(30.,0.15,-0.42));
#5594=CARTESIAN_POINT('Origin',(-0.1,0.55,-0.67));
#5595=CARTESIAN_POINT('',(0.,0.55,-0.67));
#5596=CARTESIAN_POINT('',(0.,0.245,-0.365));
#5597=CARTESIAN_POINT('',(30.,0.55,-0.67));
#5598=CARTESIAN_POINT('',(-0.1,0.55,-0.67));
#5599=CARTESIAN_POINT('',(30.,0.245,-0.365));
#5600=CARTESIAN_POINT('Origin',(-0.1,0.55,-0.82));
#5601=CARTESIAN_POINT('',(0.,0.55,-0.82));
#5602=CARTESIAN_POINT('',(0.,0.55,-0.41));
#5603=CARTESIAN_POINT('',(30.,0.55,-0.82));
#5604=CARTESIAN_POINT('',(-0.1,0.55,-0.82));
#5605=CARTESIAN_POINT('',(30.,0.55,-0.41));
#5606=CARTESIAN_POINT('Origin',(-0.1,0.3,-0.82));
#5607=CARTESIAN_POINT('',(0.,0.3,-0.82));
#5608=CARTESIAN_POINT('',(0.,0.15,-0.82));
#5609=CARTESIAN_POINT('',(30.,0.3,-0.82));
#5610=CARTESIAN_POINT('',(-0.1,0.3,-0.82));
#5611=CARTESIAN_POINT('',(30.,0.15,-0.82));
#5612=CARTESIAN_POINT('Origin',(-0.1,0.3,-1.05));
#5613=CARTESIAN_POINT('',(0.,0.3,-1.));
#5614=CARTESIAN_POINT('',(0.,0.3,-0.525));
#5615=CARTESIAN_POINT('',(30.,0.3,-1.));
#5616=CARTESIAN_POINT('',(-0.05,0.3,-1.));
#5617=CARTESIAN_POINT('',(30.,0.3,-0.525));
#5618=CARTESIAN_POINT('Origin',(-0.1,-0.82,0.3));
#5619=CARTESIAN_POINT('',(0.,-0.82,0.3));
#5620=CARTESIAN_POINT('',(0.,-1.,0.3));
#5621=CARTESIAN_POINT('',(0.,-0.41,0.3));
#5622=CARTESIAN_POINT('',(30.,-0.82,0.3));
#5623=CARTESIAN_POINT('',(-0.1,-0.82,0.3));
#5624=CARTESIAN_POINT('',(30.,-1.,0.3));
#5625=CARTESIAN_POINT('',(30.,-0.41,0.3));
#5626=CARTESIAN_POINT('',(-0.05,-1.,0.3));
#5627=CARTESIAN_POINT('Origin',(-0.1,-0.82,0.55));
#5628=CARTESIAN_POINT('',(0.,-0.82,0.55));
#5629=CARTESIAN_POINT('',(0.,-0.82,0.275));
#5630=CARTESIAN_POINT('',(30.,-0.82,0.55));
#5631=CARTESIAN_POINT('',(-0.1,-0.82,0.55));
#5632=CARTESIAN_POINT('',(30.,-0.82,0.275));
#5633=CARTESIAN_POINT('Origin',(-0.1,-0.67,0.55));
#5634=CARTESIAN_POINT('',(0.,-0.67,0.55));
#5635=CARTESIAN_POINT('',(0.,-0.335,0.55));
#5636=CARTESIAN_POINT('',(30.,-0.67,0.55));
#5637=CARTESIAN_POINT('',(-0.1,-0.67,0.55));
#5638=CARTESIAN_POINT('',(30.,-0.335,0.55));
#5639=CARTESIAN_POINT('Origin',(-0.1,-0.42,0.3));
#5640=CARTESIAN_POINT('',(0.,-0.42,0.3));
#5641=CARTESIAN_POINT('',(-6.93889390390723E-18,-0.24,0.12));
#5642=CARTESIAN_POINT('',(30.,-0.42,0.3));
#5643=CARTESIAN_POINT('',(-0.1,-0.42,0.3));
#5644=CARTESIAN_POINT('',(30.,-0.24,0.12));
#5645=CARTESIAN_POINT('Origin',(-0.1,-0.42,-0.3));
#5646=CARTESIAN_POINT('',(0.,-0.42,-0.3));
#5647=CARTESIAN_POINT('',(0.,-0.42,-0.15));
#5648=CARTESIAN_POINT('',(30.,-0.42,-0.3));
#5649=CARTESIAN_POINT('',(-0.1,-0.42,-0.3));
#5650=CARTESIAN_POINT('',(30.,-0.42,-0.15));
#5651=CARTESIAN_POINT('Origin',(-0.1,-0.67,-0.55));
#5652=CARTESIAN_POINT('',(0.,-0.67,-0.55));
#5653=CARTESIAN_POINT('',(0.,-0.365,-0.245));
#5654=CARTESIAN_POINT('',(30.,-0.67,-0.55));
#5655=CARTESIAN_POINT('',(-0.1,-0.67,-0.55));
#5656=CARTESIAN_POINT('',(30.,-0.365,-0.245));
#5657=CARTESIAN_POINT('Origin',(-0.1,-0.82,-0.55));
#5658=CARTESIAN_POINT('',(0.,-0.82,-0.55));
#5659=CARTESIAN_POINT('',(0.,-0.41,-0.55));
#5660=CARTESIAN_POINT('',(30.,-0.82,-0.55));
#5661=CARTESIAN_POINT('',(-0.1,-0.82,-0.55));
#5662=CARTESIAN_POINT('',(30.,-0.41,-0.55));
#5663=CARTESIAN_POINT('Origin',(-0.1,-0.82,-0.3));
#5664=CARTESIAN_POINT('',(0.,-0.82,-0.3));
#5665=CARTESIAN_POINT('',(0.,-0.82,-0.15));
#5666=CARTESIAN_POINT('',(30.,-0.82,-0.3));
#5667=CARTESIAN_POINT('',(-0.1,-0.82,-0.3));
#5668=CARTESIAN_POINT('',(30.,-0.82,-0.15));
#5669=CARTESIAN_POINT('Origin',(-0.1,-1.05,-0.3));
#5670=CARTESIAN_POINT('',(0.,-1.,-0.3));
#5671=CARTESIAN_POINT('',(0.,-0.525,-0.3));
#5672=CARTESIAN_POINT('',(30.,-1.,-0.3));
#5673=CARTESIAN_POINT('',(-0.05,-1.,-0.3));
#5674=CARTESIAN_POINT('',(30.,-0.525,-0.3));
#5675=CARTESIAN_POINT('Origin',(-0.1,0.3,0.82));
#5676=CARTESIAN_POINT('',(0.,0.3,0.82));
#5677=CARTESIAN_POINT('',(0.,0.3,1.));
#5678=CARTESIAN_POINT('',(0.,0.3,0.41));
#5679=CARTESIAN_POINT('',(30.,0.3,0.82));
#5680=CARTESIAN_POINT('',(-0.1,0.3,0.82));
#5681=CARTESIAN_POINT('',(30.,0.3,1.));
#5682=CARTESIAN_POINT('',(30.,0.3,0.41));
#5683=CARTESIAN_POINT('',(-0.05,0.3,1.));
#5684=CARTESIAN_POINT('Origin',(-0.1,0.55,0.82));
#5685=CARTESIAN_POINT('',(0.,0.55,0.82));
#5686=CARTESIAN_POINT('',(0.,0.275,0.82));
#5687=CARTESIAN_POINT('',(30.,0.55,0.82));
#5688=CARTESIAN_POINT('',(-0.1,0.55,0.82));
#5689=CARTESIAN_POINT('',(30.,0.275,0.82));
#5690=CARTESIAN_POINT('Origin',(-0.1,0.55,0.67));
#5691=CARTESIAN_POINT('',(0.,0.55,0.67));
#5692=CARTESIAN_POINT('',(0.,0.55,0.335));
#5693=CARTESIAN_POINT('',(30.,0.55,0.67));
#5694=CARTESIAN_POINT('',(-0.1,0.55,0.67));
#5695=CARTESIAN_POINT('',(30.,0.55,0.335));
#5696=CARTESIAN_POINT('Origin',(-0.1,0.3,0.42));
#5697=CARTESIAN_POINT('',(0.,0.3,0.42));
#5698=CARTESIAN_POINT('',(6.93889390390723E-18,0.12,0.24));
#5699=CARTESIAN_POINT('',(30.,0.3,0.42));
#5700=CARTESIAN_POINT('',(-0.1,0.3,0.42));
#5701=CARTESIAN_POINT('',(30.,0.12,0.24));
#5702=CARTESIAN_POINT('Origin',(-0.1,-0.3,0.42));
#5703=CARTESIAN_POINT('',(0.,-0.3,0.42));
#5704=CARTESIAN_POINT('',(0.,-0.15,0.42));
#5705=CARTESIAN_POINT('',(30.,-0.3,0.42));
#5706=CARTESIAN_POINT('',(-0.1,-0.3,0.42));
#5707=CARTESIAN_POINT('',(30.,-0.15,0.42));
#5708=CARTESIAN_POINT('Origin',(-0.1,-0.55,0.67));
#5709=CARTESIAN_POINT('',(0.,-0.55,0.67));
#5710=CARTESIAN_POINT('',(6.93889390390723E-18,-0.245,0.365));
#5711=CARTESIAN_POINT('',(30.,-0.55,0.67));
#5712=CARTESIAN_POINT('',(-0.1,-0.55,0.67));
#5713=CARTESIAN_POINT('',(30.,-0.245,0.365));
#5714=CARTESIAN_POINT('Origin',(-0.1,-0.55,0.82));
#5715=CARTESIAN_POINT('',(0.,-0.55,0.82));
#5716=CARTESIAN_POINT('',(0.,-0.55,0.41));
#5717=CARTESIAN_POINT('',(30.,-0.55,0.82));
#5718=CARTESIAN_POINT('',(-0.1,-0.55,0.82));
#5719=CARTESIAN_POINT('',(30.,-0.55,0.41));
#5720=CARTESIAN_POINT('Origin',(-0.1,-0.3,0.82));
#5721=CARTESIAN_POINT('',(0.,-0.3,0.82));
#5722=CARTESIAN_POINT('',(0.,-0.15,0.82));
#5723=CARTESIAN_POINT('',(30.,-0.3,0.82));
#5724=CARTESIAN_POINT('',(-0.1,-0.3,0.82));
#5725=CARTESIAN_POINT('',(30.,-0.15,0.82));
#5726=CARTESIAN_POINT('Origin',(-0.1,-0.3,1.05));
#5727=CARTESIAN_POINT('',(0.,-0.3,1.));
#5728=CARTESIAN_POINT('',(0.,-0.3,0.525));
#5729=CARTESIAN_POINT('',(30.,-0.3,1.));
#5730=CARTESIAN_POINT('',(-0.05,-0.3,1.));
#5731=CARTESIAN_POINT('',(30.,-0.3,0.525));
#5732=CARTESIAN_POINT('Origin',(-0.1,0.,0.));
#5733=CARTESIAN_POINT('',(0.,-2.57175827820944E-17,0.21));
#5734=CARTESIAN_POINT('Origin',(0.,0.,0.));
#5735=CARTESIAN_POINT('',(30.,2.57175827820944E-17,0.21));
#5736=CARTESIAN_POINT('',(-0.1,-2.57175827820944E-17,0.21));
#5737=CARTESIAN_POINT('Origin',(30.,0.,0.));
#5738=CARTESIAN_POINT('Origin',(0.,1.,-1.));
#5739=CARTESIAN_POINT('',(0.,1.,1.));
#5740=CARTESIAN_POINT('',(0.,1.,-1.));
#5741=CARTESIAN_POINT('',(30.,1.,1.));
#5742=CARTESIAN_POINT('',(0.,1.,1.));
#5743=CARTESIAN_POINT('',(30.,1.,-1.));
#5744=CARTESIAN_POINT('Origin',(0.,1.,-1.));
#5745=CARTESIAN_POINT('',(30.,1.,-1.));
#5746=CARTESIAN_POINT('',(30.,1.,-1.));
#5747=CARTESIAN_POINT('',(0.,1.,-1.));
#5748=CARTESIAN_POINT('',(0.,1.,-1.));
#5749=CARTESIAN_POINT('',(0.,1.,-1.));
#5750=CARTESIAN_POINT('Origin',(0.,-1.,-1.));
#5751=CARTESIAN_POINT('',(0.,-1.,-1.));
#5752=CARTESIAN_POINT('',(30.,-1.,-1.));
#5753=CARTESIAN_POINT('Origin',(0.,-1.,-1.));
#5754=CARTESIAN_POINT('',(30.,-1.,-1.));
#5755=CARTESIAN_POINT('',(30.,-1.,-1.));
#5756=CARTESIAN_POINT('',(0.,-1.,-1.));
#5757=CARTESIAN_POINT('',(0.,-1.,-1.));
#5758=CARTESIAN_POINT('',(0.,-1.,-1.));
#5759=CARTESIAN_POINT('Origin',(0.,-1.,1.));
#5760=CARTESIAN_POINT('',(0.,-1.,1.));
#5761=CARTESIAN_POINT('',(30.,-1.,1.));
#5762=CARTESIAN_POINT('Origin',(0.,-1.,1.));
#5763=CARTESIAN_POINT('',(30.,-1.,1.));
#5764=CARTESIAN_POINT('',(30.,-1.,1.));
#5765=CARTESIAN_POINT('',(0.,-1.,1.));
#5766=CARTESIAN_POINT('',(0.,-1.,1.));
#5767=CARTESIAN_POINT('',(0.,-1.,1.));
#5768=CARTESIAN_POINT('Origin',(0.,1.,1.));
#5769=CARTESIAN_POINT('',(0.,1.,1.));
#5770=CARTESIAN_POINT('',(30.,1.,1.));
#5771=CARTESIAN_POINT('Origin',(0.,1.,1.));
#5772=CARTESIAN_POINT('',(30.,1.,1.));
#5773=CARTESIAN_POINT('',(0.,1.,1.));
#5774=CARTESIAN_POINT('Origin',(30.,0.,0.));
#5775=CARTESIAN_POINT('Origin',(0.,0.,0.));
#5776=CARTESIAN_POINT('',(0.,0.,0.));
#5777=CARTESIAN_POINT('Origin',(0.,-2.1,6.));
#5778=CARTESIAN_POINT('',(-0.275,-1.8,6.));
#5779=CARTESIAN_POINT('Origin',(0.,-1.8,6.));
#5780=CARTESIAN_POINT('',(-0.275,-1.,6.));
#5781=CARTESIAN_POINT('',(-0.275,-2.1,6.));
#5782=CARTESIAN_POINT('Origin',(0.,-1.,6.));
#5783=CARTESIAN_POINT('Origin',(0.,-2.1,7.2));
#5784=CARTESIAN_POINT('',(-0.275,-1.8,7.2));
#5785=CARTESIAN_POINT('Origin',(0.,-1.8,7.2));
#5786=CARTESIAN_POINT('',(-0.275,-1.,7.2));
#5787=CARTESIAN_POINT('',(-0.275,-2.1,7.2));
#5788=CARTESIAN_POINT('Origin',(0.,-1.,7.2));
#5789=CARTESIAN_POINT('Origin',(2.,-1.8,5.4));
#5790=CARTESIAN_POINT('',(1.69,-1.8,5.5));
#5791=CARTESIAN_POINT('Origin',(2.,-1.8,5.5));
#5792=CARTESIAN_POINT('',(1.69,-1.8,6.));
#5793=CARTESIAN_POINT('',(1.69,-1.8,5.4));
#5794=CARTESIAN_POINT('Origin',(2.,-1.8,6.));
#5795=CARTESIAN_POINT('Origin',(2.,-1.8,5.4));
#5796=CARTESIAN_POINT('',(1.69,-1.8,7.2));
#5797=CARTESIAN_POINT('Origin',(2.,-1.8,7.2));
#5798=CARTESIAN_POINT('',(1.69,-1.8,7.7));
#5799=CARTESIAN_POINT('',(1.69,-1.8,5.4));
#5800=CARTESIAN_POINT('Origin',(2.,-1.8,7.7));
#5801=CARTESIAN_POINT('Origin',(1.38,-1.1,6.));
#5802=CARTESIAN_POINT('',(1.38,-1.8,6.));
#5803=CARTESIAN_POINT('',(1.38,-1.8,7.2));
#5804=CARTESIAN_POINT('',(1.38,-1.8,5.75));
#5805=CARTESIAN_POINT('',(1.38,-1.1,6.));
#5806=CARTESIAN_POINT('',(1.38,-1.1,6.));
#5807=CARTESIAN_POINT('',(1.38,-1.1,7.2));
#5808=CARTESIAN_POINT('',(1.38,-1.1,6.));
#5809=CARTESIAN_POINT('',(1.38,-1.1,7.2));
#5810=CARTESIAN_POINT('Origin',(2.7,-1.1,6.));
#5811=CARTESIAN_POINT('',(1.6,-1.1,7.2));
#5812=CARTESIAN_POINT('',(1.6,-1.1,6.));
#5813=CARTESIAN_POINT('',(1.6,-1.1,5.75));
#5814=CARTESIAN_POINT('',(2.7,-1.1,7.2));
#5815=CARTESIAN_POINT('',(2.7,-1.1,6.));
#5816=CARTESIAN_POINT('Origin',(-1.,-1.8,5.5));
#5817=CARTESIAN_POINT('',(1.4,-1.8,6.));
#5818=CARTESIAN_POINT('',(0.52,-1.8,6.));
#5819=CARTESIAN_POINT('',(1.4,-1.8,7.2));
#5820=CARTESIAN_POINT('',(0.52,-1.8,7.2));
#5821=CARTESIAN_POINT('',(1.4,-1.8,7.7));
#5822=CARTESIAN_POINT('',(1.4,-1.8,7.2));
#5823=CARTESIAN_POINT('',(-1.,-1.8,7.7));
#5824=CARTESIAN_POINT('',(-1.,-1.8,7.7));
#5825=CARTESIAN_POINT('',(-1.,-1.8,5.5));
#5826=CARTESIAN_POINT('',(-1.,-1.8,5.5));
#5827=CARTESIAN_POINT('',(1.4,-1.8,5.5));
#5828=CARTESIAN_POINT('',(-1.,-1.8,5.5));
#5829=CARTESIAN_POINT('',(1.4,-1.8,5.5));
#5830=CARTESIAN_POINT('Origin',(2.,-1.8,7.2));
#5831=CARTESIAN_POINT('',(1.6,-1.35278640450004,7.7));
#5832=CARTESIAN_POINT('',(1.6,-1.35278640450004,7.2));
#5833=CARTESIAN_POINT('',(1.6,-1.35278640450004,7.2));
#5834=CARTESIAN_POINT('Origin',(2.,-1.8,7.7));
#5835=CARTESIAN_POINT('Origin',(2.,-1.8,7.2));
#5836=CARTESIAN_POINT('Origin',(2.,-1.8,7.2));
#5837=CARTESIAN_POINT('',(1.6,-1.8,7.2));
#5838=CARTESIAN_POINT('Origin',(1.6,-1.8,5.5));
#5839=CARTESIAN_POINT('',(1.6,-1.35278640450004,6.));
#5840=CARTESIAN_POINT('',(1.6,-1.8,6.));
#5841=CARTESIAN_POINT('',(1.6,-1.35278640450004,5.5));
#5842=CARTESIAN_POINT('',(1.6,-1.35278640450004,5.5));
#5843=CARTESIAN_POINT('',(1.6,-1.,5.5));
#5844=CARTESIAN_POINT('',(1.6,-1.8,5.5));
#5845=CARTESIAN_POINT('',(1.6,-1.,7.7));
#5846=CARTESIAN_POINT('',(1.6,-1.,5.5));
#5847=CARTESIAN_POINT('',(1.6,-1.8,7.7));
#5848=CARTESIAN_POINT('Origin',(2.,-1.8,6.));
#5849=CARTESIAN_POINT('Origin',(2.,-1.8,6.));
#5850=CARTESIAN_POINT('Origin',(2.,-1.8,5.5));
#5851=CARTESIAN_POINT('Origin',(2.,-1.8,5.5));
#5852=CARTESIAN_POINT('Origin',(0.3,-1.4,5.5));
#5853=CARTESIAN_POINT('',(-1.,-1.,5.5));
#5854=CARTESIAN_POINT('',(-1.,-1.,5.5));
#5855=CARTESIAN_POINT('',(1.6,-1.,5.5));
#5856=CARTESIAN_POINT('Origin',(1.6,-1.,5.5));
#5857=CARTESIAN_POINT('',(-1.,-1.,7.7));
#5858=CARTESIAN_POINT('',(-1.,-1.,5.5));
#5859=CARTESIAN_POINT('',(1.6,-1.,7.7));
#5860=CARTESIAN_POINT('Origin',(-1.,-1.,5.5));
#5861=CARTESIAN_POINT('',(-1.,-1.,7.7));
#5862=CARTESIAN_POINT('Origin',(0.3,-1.4,7.7));
#5863=CARTESIAN_POINT('',(0.,0.,0.));
#5864=CARTESIAN_POINT('Origin',(0.,-2.7,0.));
#5865=CARTESIAN_POINT('',(-0.289136645896019,-2.7,0.08));
#5866=CARTESIAN_POINT('',(-0.3,-2.78,-2.27065106771523E-17));
#5867=CARTESIAN_POINT('Ctrl Pts',(-0.289136645896019,-2.7,0.08));
#5868=CARTESIAN_POINT('Ctrl Pts',(-0.289136645896019,-2.71009877520201,
0.08));
#5869=CARTESIAN_POINT('Ctrl Pts',(-0.289720927595908,-2.72083518625944,
0.0779717130936404));
#5870=CARTESIAN_POINT('Ctrl Pts',(-0.291799203044223,-2.74052980652726,
0.0697927537456149));
#5871=CARTESIAN_POINT('Ctrl Pts',(-0.293259762986909,-2.74949254880105,
0.0636445361887959));
#5872=CARTESIAN_POINT('Ctrl Pts',(-0.295976783522942,-2.76364324458222,
0.0494938404076284));
#5873=CARTESIAN_POINT('Ctrl Pts',(-0.297414335384467,-2.76979246713824,
0.0405305642602551));
#5874=CARTESIAN_POINT('Ctrl Pts',(-0.299439403644655,-2.77797216257078,
0.0208340363410407));
#5875=CARTESIAN_POINT('Ctrl Pts',(-0.3,-2.78,0.0100969318362556));
#5876=CARTESIAN_POINT('Ctrl Pts',(-0.3,-2.78,5.20417042793042E-18));
#5877=CARTESIAN_POINT('',(0.289136645896019,-2.7,0.08));
#5878=CARTESIAN_POINT('',(0.,-2.7,0.08));
#5879=CARTESIAN_POINT('Ctrl Pts',(0.289136645896019,-2.7,0.08));
#5880=CARTESIAN_POINT('Ctrl Pts',(0.289136645896019,-2.68990122479799,0.08));
#5881=CARTESIAN_POINT('Ctrl Pts',(0.289720927595908,-2.67916481374056,0.0779717130936404));
#5882=CARTESIAN_POINT('Ctrl Pts',(0.291799203044223,-2.65947019347274,0.0697927537456147));
#5883=CARTESIAN_POINT('Ctrl Pts',(0.293259762986909,-2.65050745119895,0.0636445361887959));
#5884=CARTESIAN_POINT('Ctrl Pts',(0.295976783522942,-2.63635675541778,0.0494938404076283));
#5885=CARTESIAN_POINT('Ctrl Pts',(0.297414335384467,-2.63020753286176,0.0405305642602551));
#5886=CARTESIAN_POINT('Ctrl Pts',(0.299439403644655,-2.62202783742922,0.0208340363410406));
#5887=CARTESIAN_POINT('Ctrl Pts',(0.3,-2.62,0.0100969318362555));
#5888=CARTESIAN_POINT('Ctrl Pts',(0.3,-2.62,-0.0100969318362556));
#5889=CARTESIAN_POINT('Ctrl Pts',(0.299439403644655,-2.62202783742922,-0.0208340363410406));
#5890=CARTESIAN_POINT('Ctrl Pts',(0.297414335384467,-2.63020753286176,-0.0405305642602551));
#5891=CARTESIAN_POINT('Ctrl Pts',(0.295976783522942,-2.63635675541778,-0.0494938404076283));
#5892=CARTESIAN_POINT('Ctrl Pts',(0.293259762986909,-2.65050745119895,-0.0636445361887959));
#5893=CARTESIAN_POINT('Ctrl Pts',(0.291799203044223,-2.65947019347274,-0.0697927537456147));
#5894=CARTESIAN_POINT('Ctrl Pts',(0.289720927595908,-2.67916481374056,-0.0779717130936403));
#5895=CARTESIAN_POINT('Ctrl Pts',(0.289136645896019,-2.68990122479799,-0.08));
#5896=CARTESIAN_POINT('Ctrl Pts',(0.289136645896019,-2.71009877520201,-0.08));
#5897=CARTESIAN_POINT('Ctrl Pts',(0.289720927595908,-2.72083518625944,-0.0779717130936404));
#5898=CARTESIAN_POINT('Ctrl Pts',(0.291799203044223,-2.74052980652726,-0.0697927537456147));
#5899=CARTESIAN_POINT('Ctrl Pts',(0.293259762986909,-2.74949254880105,-0.0636445361887959));
#5900=CARTESIAN_POINT('Ctrl Pts',(0.295976783522942,-2.76364324458222,-0.0494938404076283));
#5901=CARTESIAN_POINT('Ctrl Pts',(0.297414335384467,-2.76979246713824,-0.0405305642602551));
#5902=CARTESIAN_POINT('Ctrl Pts',(0.299439403644655,-2.77797216257078,-0.0208340363410406));
#5903=CARTESIAN_POINT('Ctrl Pts',(0.3,-2.78,-0.0100969318362555));
#5904=CARTESIAN_POINT('Ctrl Pts',(0.3,-2.78,0.0100969318362556));
#5905=CARTESIAN_POINT('Ctrl Pts',(0.299439403644655,-2.77797216257078,0.0208340363410407));
#5906=CARTESIAN_POINT('Ctrl Pts',(0.297414335384467,-2.76979246713824,0.0405305642602551));
#5907=CARTESIAN_POINT('Ctrl Pts',(0.295976783522942,-2.76364324458222,0.0494938404076284));
#5908=CARTESIAN_POINT('Ctrl Pts',(0.293259762986909,-2.74949254880105,0.0636445361887959));
#5909=CARTESIAN_POINT('Ctrl Pts',(0.291799203044223,-2.74052980652726,0.0697927537456149));
#5910=CARTESIAN_POINT('Ctrl Pts',(0.289720927595908,-2.72083518625944,0.0779717130936404));
#5911=CARTESIAN_POINT('Ctrl Pts',(0.289136645896019,-2.71009877520201,0.08));
#5912=CARTESIAN_POINT('Ctrl Pts',(0.289136645896019,-2.7,0.08));
#5913=CARTESIAN_POINT('',(-0.3,-2.62,-3.65842984849668E-17));
#5914=CARTESIAN_POINT('Ctrl Pts',(-0.3,-2.62,-3.81639164714898E-17));
#5915=CARTESIAN_POINT('Ctrl Pts',(-0.3,-2.62,0.0100969318362555));
#5916=CARTESIAN_POINT('Ctrl Pts',(-0.299439403644655,-2.62202783742922,
0.0208340363410406));
#5917=CARTESIAN_POINT('Ctrl Pts',(-0.297414335384467,-2.63020753286176,
0.040530564260255));
#5918=CARTESIAN_POINT('Ctrl Pts',(-0.295976783522942,-2.63635675541778,
0.0494938404076283));
#5919=CARTESIAN_POINT('Ctrl Pts',(-0.293259762986909,-2.65050745119895,
0.0636445361887959));
#5920=CARTESIAN_POINT('Ctrl Pts',(-0.291799203044223,-2.65947019347274,
0.0697927537456147));
#5921=CARTESIAN_POINT('Ctrl Pts',(-0.289720927595908,-2.67916481374056,
0.0779717130936404));
#5922=CARTESIAN_POINT('Ctrl Pts',(-0.289136645896019,-2.68990122479799,
0.08));
#5923=CARTESIAN_POINT('Ctrl Pts',(-0.289136645896019,-2.7,0.08));
#5924=CARTESIAN_POINT('Ctrl Pts',(-0.3,-2.78,-6.93889390390723E-18));
#5925=CARTESIAN_POINT('Ctrl Pts',(-0.3,-2.78,-0.0100969318362556));
#5926=CARTESIAN_POINT('Ctrl Pts',(-0.299439403644655,-2.77797216257078,
-0.0208340363410406));
#5927=CARTESIAN_POINT('Ctrl Pts',(-0.297414335384467,-2.76979246713824,
-0.0405305642602551));
#5928=CARTESIAN_POINT('Ctrl Pts',(-0.295976783522942,-2.76364324458222,
-0.0494938404076283));
#5929=CARTESIAN_POINT('Ctrl Pts',(-0.293259762986909,-2.74949254880105,
-0.0636445361887959));
#5930=CARTESIAN_POINT('Ctrl Pts',(-0.291799203044223,-2.74052980652726,
-0.0697927537456147));
#5931=CARTESIAN_POINT('Ctrl Pts',(-0.289720927595908,-2.72083518625944,
-0.0779717130936403));
#5932=CARTESIAN_POINT('Ctrl Pts',(-0.289136645896019,-2.71009877520201,
-0.08));
#5933=CARTESIAN_POINT('Ctrl Pts',(-0.289136645896019,-2.68990122479799,
-0.08));
#5934=CARTESIAN_POINT('Ctrl Pts',(-0.289720927595908,-2.67916481374056,
-0.0779717130936403));
#5935=CARTESIAN_POINT('Ctrl Pts',(-0.291799203044223,-2.65947019347274,
-0.0697927537456147));
#5936=CARTESIAN_POINT('Ctrl Pts',(-0.293259762986909,-2.65050745119895,
-0.0636445361887959));
#5937=CARTESIAN_POINT('Ctrl Pts',(-0.295976783522942,-2.63635675541778,
-0.0494938404076283));
#5938=CARTESIAN_POINT('Ctrl Pts',(-0.297414335384467,-2.63020753286176,
-0.0405305642602551));
#5939=CARTESIAN_POINT('Ctrl Pts',(-0.299439403644655,-2.62202783742922,
-0.0208340363410406));
#5940=CARTESIAN_POINT('Ctrl Pts',(-0.3,-2.62,-0.0100969318362556));
#5941=CARTESIAN_POINT('Ctrl Pts',(-0.3,-2.62,-1.56125112837913E-17));
#5942=CARTESIAN_POINT('Origin',(0.45,0.2,0.));
#5943=CARTESIAN_POINT('',(-0.45,0.2,-5.51091059616309E-17));
#5944=CARTESIAN_POINT('Origin',(0.,0.2,0.));
#5945=CARTESIAN_POINT('Origin',(0.,0.175,0.));
#5946=CARTESIAN_POINT('',(-0.5,0.15,-6.12323399573676E-17));
#5947=CARTESIAN_POINT('Origin',(0.,0.15,0.));
#5948=CARTESIAN_POINT('',(-0.475,0.175,-5.81707229594993E-17));
#5949=CARTESIAN_POINT('Origin',(0.,0.0750000000000002,0.));
#5950=CARTESIAN_POINT('',(-0.5,0.,-6.12323399573677E-17));
#5951=CARTESIAN_POINT('Origin',(0.,0.,0.));
#5952=CARTESIAN_POINT('',(-0.5,0.0750000000000002,-6.12323399573677E-17));
#5953=CARTESIAN_POINT('Origin',(0.3,0.,0.));
#5954=CARTESIAN_POINT('',(-0.3,0.,-3.67394039744206E-17));
#5955=CARTESIAN_POINT('Origin',(0.,0.,0.));
#5956=CARTESIAN_POINT('Origin',(0.,-1.455,0.));
#5957=CARTESIAN_POINT('',(-0.3,-2.91,-3.67394039744206E-17));
#5958=CARTESIAN_POINT('Origin',(0.,-2.91,0.));
#5959=CARTESIAN_POINT('',(-0.3,-1.455,-3.67394039744206E-17));
#5960=CARTESIAN_POINT('',(-0.3,-1.455,-3.67394039744206E-17));
#5961=CARTESIAN_POINT('Origin',(0.,-2.955,0.));
#5962=CARTESIAN_POINT('',(-0.21,-3.,-2.57175827820944E-17));
#5963=CARTESIAN_POINT('Origin',(0.,-3.,0.));
#5964=CARTESIAN_POINT('',(-0.255,-2.955,-3.12284933782575E-17));
#5965=CARTESIAN_POINT('Origin',(0.,-3.,0.));
#5966=CARTESIAN_POINT('',(0.,0.,0.));
#5967=CARTESIAN_POINT('Origin',(0.,0.,0.));
#5968=CARTESIAN_POINT('',(-0.32,0.16,3.91886975727153E-17));
#5969=CARTESIAN_POINT('Origin',(0.,0.16,0.));
#5970=CARTESIAN_POINT('',(-0.32,0.,3.91886975727153E-17));
#5971=CARTESIAN_POINT('',(-0.32,0.,3.91886975727153E-17));
#5972=CARTESIAN_POINT('Origin',(0.,0.,0.));
#5973=CARTESIAN_POINT('Origin',(0.,0.,0.));
#5974=CARTESIAN_POINT('',(-0.6,0.16,7.34788079488412E-17));
#5975=CARTESIAN_POINT('Origin',(0.,0.16,0.));
#5976=CARTESIAN_POINT('',(-0.6,0.,7.34788079488412E-17));
#5977=CARTESIAN_POINT('',(-0.6,0.,7.34788079488412E-17));
#5978=CARTESIAN_POINT('Origin',(0.,0.,0.));
#5979=CARTESIAN_POINT('Origin',(0.,0.16,0.));
#5980=CARTESIAN_POINT('Origin',(0.,0.,0.));
#5981=CARTESIAN_POINT('',(0.,0.,0.));
#5982=CARTESIAN_POINT('Origin',(0.,0.12,0.));
#5983=CARTESIAN_POINT('',(-9.79717439317883E-18,0.12,-0.04));
#5984=CARTESIAN_POINT('Origin',(0.,0.12,-0.12));
#5985=CARTESIAN_POINT('Origin',(9.79717439317883E-18,0.12,0.));
#5986=CARTESIAN_POINT('',(0.08,-4.89858719658941E-18,7.34788079488412E-18));
#5987=CARTESIAN_POINT('',(-0.08,-4.89858719658941E-18,7.34788079488412E-18));
#5988=CARTESIAN_POINT('Ctrl Pts',(0.08,-4.89858719658941E-18,7.34788079488412E-18));
#5989=CARTESIAN_POINT('Ctrl Pts',(0.08,-0.00012864962353541,0.000128649623535413));
#5990=CARTESIAN_POINT('Ctrl Pts',(0.0799996896739287,-0.00025719571182076,
0.000257402596003253));
#5991=CARTESIAN_POINT('Ctrl Pts',(0.0799669711262291,-0.00701193164572964,
0.00703384588894362));
#5992=CARTESIAN_POINT('Ctrl Pts',(0.0791054994909294,-0.0133457972655825,
0.0139383126556792));
#5993=CARTESIAN_POINT('Ctrl Pts',(0.0749700088488058,-0.0265076530862524,
0.0292212026164895));
#5994=CARTESIAN_POINT('Ctrl Pts',(0.0712702072865517,-0.0331317062461458,
0.0375603420117568));
#5995=CARTESIAN_POINT('Ctrl Pts',(0.0612858949407667,-0.0440683985740427,
0.0520545604187517));
#5996=CARTESIAN_POINT('Ctrl Pts',(0.0555090276731744,-0.0485199197794574,
0.0582717815295611));
#5997=CARTESIAN_POINT('Ctrl Pts',(0.0412398082144208,-0.0561090538733877,
0.0691638397919718));
#5998=CARTESIAN_POINT('Ctrl Pts',(0.0327878980890048,-0.059089642483296,
0.0736229049587921));
#5999=CARTESIAN_POINT('Ctrl Pts',(0.0159233027310102,-0.0625179833270725,
0.0787936360751706));
#6000=CARTESIAN_POINT('Ctrl Pts',(0.00801661414593076,-0.0633030277982336,
0.08));
#6001=CARTESIAN_POINT('Ctrl Pts',(-0.00801661414593074,-0.0633030277982336,
0.08));
#6002=CARTESIAN_POINT('Ctrl Pts',(-0.0159233027310102,-0.0625179833270726,
0.0787936360751706));
#6003=CARTESIAN_POINT('Ctrl Pts',(-0.0327878980890049,-0.059089642483296,
0.0736229049587921));
#6004=CARTESIAN_POINT('Ctrl Pts',(-0.0412398082144209,-0.0561090538733877,
0.0691638397919717));
#6005=CARTESIAN_POINT('Ctrl Pts',(-0.0555090276731744,-0.0485199197794574,
0.0582717815295611));
#6006=CARTESIAN_POINT('Ctrl Pts',(-0.0612858949407667,-0.0440683985740427,
0.0520545604187517));
#6007=CARTESIAN_POINT('Ctrl Pts',(-0.0712702072865517,-0.0331317062461458,
0.0375603420117568));
#6008=CARTESIAN_POINT('Ctrl Pts',(-0.0749700088488058,-0.0265076530862524,
0.0292212026164895));
#6009=CARTESIAN_POINT('Ctrl Pts',(-0.0791054994909264,-0.0133457972655921,
0.0139383126556903));
#6010=CARTESIAN_POINT('Ctrl Pts',(-0.0799669711262287,-0.00701193164579759,
0.0070338458890125));
#6011=CARTESIAN_POINT('Ctrl Pts',(-0.0799996896739287,-0.000257195711817665,
0.000257402596000083));
#6012=CARTESIAN_POINT('Ctrl Pts',(-0.08,-0.000128649623538514,0.000128649623538516));
#6013=CARTESIAN_POINT('Ctrl Pts',(-0.08,-4.89858719658941E-18,7.34788079488412E-18));
#6014=CARTESIAN_POINT('Ctrl Pts',(-0.08,-4.89858719658941E-18,7.34788079488412E-18));
#6015=CARTESIAN_POINT('Ctrl Pts',(-0.08,-0.000128649623536042,-0.00012864962353603));
#6016=CARTESIAN_POINT('Ctrl Pts',(-0.0799996896739287,-0.000257195711820127,
-0.000257402596002604));
#6017=CARTESIAN_POINT('Ctrl Pts',(-0.0799669711262289,-0.0070119316457589,
-0.00703384588897312));
#6018=CARTESIAN_POINT('Ctrl Pts',(-0.0791054994909281,-0.0133457972655867,
-0.0139383126556841));
#6019=CARTESIAN_POINT('Ctrl Pts',(-0.0749700088488058,-0.0265076530862525,
-0.0292212026164896));
#6020=CARTESIAN_POINT('Ctrl Pts',(-0.0712702072865516,-0.0331317062461459,
-0.0375603420117568));
#6021=CARTESIAN_POINT('Ctrl Pts',(-0.0612858949407667,-0.0440683985740427,
-0.0520545604187517));
#6022=CARTESIAN_POINT('Ctrl Pts',(-0.0555090276731744,-0.0485199197794574,
-0.0582717815295611));
#6023=CARTESIAN_POINT('Ctrl Pts',(-0.0412398082144209,-0.0561090538733877,
-0.0691638397919717));
#6024=CARTESIAN_POINT('Ctrl Pts',(-0.0327878980890049,-0.059089642483296,
-0.0736229049587921));
#6025=CARTESIAN_POINT('Ctrl Pts',(-0.0159233027310101,-0.0625179833270725,
-0.0787936360751706));
#6026=CARTESIAN_POINT('Ctrl Pts',(-0.00801661414593069,-0.0633030277982336,
-0.08));
#6027=CARTESIAN_POINT('Ctrl Pts',(0.0080166141459307,-0.0633030277982336,
-0.08));
#6028=CARTESIAN_POINT('Ctrl Pts',(0.0159233027310101,-0.0625179833270725,
-0.0787936360751706));
#6029=CARTESIAN_POINT('Ctrl Pts',(0.0327878980890049,-0.0590896424832959,
-0.0736229049587921));
#6030=CARTESIAN_POINT('Ctrl Pts',(0.0412398082144209,-0.0561090538733877,
-0.0691638397919717));
#6031=CARTESIAN_POINT('Ctrl Pts',(0.0555090276731744,-0.0485199197794574,
-0.0582717815295611));
#6032=CARTESIAN_POINT('Ctrl Pts',(0.0612858949407666,-0.0440683985740428,
-0.0520545604187518));
#6033=CARTESIAN_POINT('Ctrl Pts',(0.0712702072865517,-0.0331317062461458,
-0.0375603420117568));
#6034=CARTESIAN_POINT('Ctrl Pts',(0.0749700088488058,-0.0265076530862524,
-0.0292212026164895));
#6035=CARTESIAN_POINT('Ctrl Pts',(0.079105499490928,-0.013345797265587,
-0.0139383126556845));
#6036=CARTESIAN_POINT('Ctrl Pts',(0.0799669711262289,-0.00701193164576148,
-0.00703384588897579));
#6037=CARTESIAN_POINT('Ctrl Pts',(0.0799996896739287,-0.000257195711819584,
-0.000257402596002039));
#6038=CARTESIAN_POINT('Ctrl Pts',(0.08,-0.000128649623536605,-0.000128649623536593));
#6039=CARTESIAN_POINT('Ctrl Pts',(0.08,-4.89858719658941E-18,7.34788079488412E-18));
#6040=CARTESIAN_POINT('Origin',(0.04,-1.36,0.));
#6041=CARTESIAN_POINT('',(0.,-1.36,-0.08));
#6042=CARTESIAN_POINT('',(0.,-1.36,0.08));
#6043=CARTESIAN_POINT('Origin',(0.,-1.36,0.));
#6044=CARTESIAN_POINT('',(0.,-1.36,-0.04));
#6045=CARTESIAN_POINT('Origin',(0.,0.,-0.08));
#6046=CARTESIAN_POINT('',(0.,-1.6,0.08));
#6047=CARTESIAN_POINT('',(0.,0.,0.08));
#6048=CARTESIAN_POINT('',(0.,-1.6,-0.08));
#6049=CARTESIAN_POINT('',(0.,-1.6,-0.09));
#6050=CARTESIAN_POINT('',(0.,0.,-0.08));
#6051=CARTESIAN_POINT('Origin',(0.,0.,0.));
#6052=CARTESIAN_POINT('',(-0.08,-1.6,-9.79717439317883E-18));
#6053=CARTESIAN_POINT('Origin',(0.,-1.6,0.));
#6054=CARTESIAN_POINT('',(-0.08,0.,-9.79717439317883E-18));
#6055=CARTESIAN_POINT('Origin',(0.,-1.6,0.));
#6056=CARTESIAN_POINT('Origin',(-0.04,-1.6,0.));
#6057=CARTESIAN_POINT('',(0.,0.,0.));
#6058=CARTESIAN_POINT('Origin',(-0.25,-0.225,0.075));
#6059=CARTESIAN_POINT('',(0.5,-0.15,0.));
#6060=CARTESIAN_POINT('',(0.5,-0.3,0.15));
#6061=CARTESIAN_POINT('',(0.5,-0.225,0.075));
#6062=CARTESIAN_POINT('',(-0.5,-0.3,0.15));
#6063=CARTESIAN_POINT('',(-0.25,-0.3,0.15));
#6064=CARTESIAN_POINT('',(-0.5,-0.15,0.));
#6065=CARTESIAN_POINT('',(-0.5,-0.075,-0.075));
#6066=CARTESIAN_POINT('',(-0.149388386429468,-0.15,0.));
#6067=CARTESIAN_POINT('',(-0.25,-0.15,0.));
#6068=CARTESIAN_POINT('',(0.149388386429468,-0.15,0.));
#6069=CARTESIAN_POINT('Origin',(0.,0.,-0.15));
#6070=CARTESIAN_POINT('',(-0.25,-0.15,0.));
#6071=CARTESIAN_POINT('Origin',(0.,0.,-0.1));
#6072=CARTESIAN_POINT('',(-0.2117,-2.59257727379495E-17,0.));
#6073=CARTESIAN_POINT('Origin',(0.,0.,0.));
#6074=CARTESIAN_POINT('',(-0.2117,2.59257727379495E-17,0.4));
#6075=CARTESIAN_POINT('',(-0.2117,-2.59257727379495E-17,-0.1));
#6076=CARTESIAN_POINT('Origin',(0.,0.,0.4));
#6077=CARTESIAN_POINT('',(-0.149388386429468,0.15,0.));
#6078=CARTESIAN_POINT('Origin',(0.,0.,0.));
#6079=CARTESIAN_POINT('',(0.149388386429468,0.15,0.));
#6080=CARTESIAN_POINT('Origin',(0.,0.,-0.15));
#6081=CARTESIAN_POINT('Origin',(0.,0.,0.));
#6082=CARTESIAN_POINT('Origin',(0.,0.,0.));
#6083=CARTESIAN_POINT('',(-0.5,0.15,0.));
#6084=CARTESIAN_POINT('',(-0.5,0.3,0.));
#6085=CARTESIAN_POINT('',(0.25,0.15,0.));
#6086=CARTESIAN_POINT('Origin',(0.,0.,0.));
#6087=CARTESIAN_POINT('',(0.5,0.15,0.));
#6088=CARTESIAN_POINT('',(0.25,0.15,0.));
#6089=CARTESIAN_POINT('',(0.5,-0.3,0.));
#6090=CARTESIAN_POINT('Origin',(0.25,0.225,0.075));
#6091=CARTESIAN_POINT('',(-0.5,0.3,0.15));
#6092=CARTESIAN_POINT('',(-0.5,0.225,0.075));
#6093=CARTESIAN_POINT('',(0.5,0.3,0.15));
#6094=CARTESIAN_POINT('',(0.25,0.3,0.15));
#6095=CARTESIAN_POINT('',(0.5,0.075,-0.075));
#6096=CARTESIAN_POINT('Origin',(0.5,-0.3,0.));
#6097=CARTESIAN_POINT('',(0.5,0.3,0.4));
#6098=CARTESIAN_POINT('',(0.5,0.3,0.));
#6099=CARTESIAN_POINT('',(0.5,-0.3,0.4));
#6100=CARTESIAN_POINT('',(0.5,-0.3,0.4));
#6101=CARTESIAN_POINT('',(0.5,-0.3,0.));
#6102=CARTESIAN_POINT('Origin',(0.5,0.3,0.));
#6103=CARTESIAN_POINT('',(-0.5,0.3,0.4));
#6104=CARTESIAN_POINT('',(-0.5,0.3,0.));
#6105=CARTESIAN_POINT('',(0.5,0.3,0.4));
#6106=CARTESIAN_POINT('Origin',(-0.5,-0.3,0.));
#6107=CARTESIAN_POINT('',(-0.5,-0.3,0.4));
#6108=CARTESIAN_POINT('',(-0.5,-0.3,0.4));
#6109=CARTESIAN_POINT('',(-0.5,-0.3,0.));
#6110=CARTESIAN_POINT('Origin',(-0.5,0.3,0.));
#6111=CARTESIAN_POINT('',(-0.5,0.3,0.4));
#6112=CARTESIAN_POINT('Origin',(0.,0.,0.4));
#6113=CARTESIAN_POINT('',(0.,0.,0.));
#6114=CARTESIAN_POINT('Origin',(0.115470053837925,-0.5,-0.2));
#6115=CARTESIAN_POINT('',(0.23094010767585,-0.5,0.));
#6116=CARTESIAN_POINT('',(0.115470053837925,-0.5,-0.2));
#6117=CARTESIAN_POINT('',(0.23094010767585,-0.5,0.));
#6118=CARTESIAN_POINT('',(0.115470053837925,-0.8,-0.2));
#6119=CARTESIAN_POINT('',(0.115470053837925,-0.5,-0.2));
#6120=CARTESIAN_POINT('',(0.23094010767585,-0.8,0.));
#6121=CARTESIAN_POINT('',(0.23094010767585,-0.8,0.));
#6122=CARTESIAN_POINT('',(0.23094010767585,-0.5,0.));
#6123=CARTESIAN_POINT('Origin',(-0.115470053837925,-0.5,-0.2));
#6124=CARTESIAN_POINT('',(-0.115470053837925,-0.5,-0.2));
#6125=CARTESIAN_POINT('',(0.115470053837925,-0.5,-0.2));
#6126=CARTESIAN_POINT('',(-0.115470053837925,-0.8,-0.2));
#6127=CARTESIAN_POINT('',(-0.115470053837925,-0.5,-0.2));
#6128=CARTESIAN_POINT('',(0.115470053837925,-0.8,-0.2));
#6129=CARTESIAN_POINT('Origin',(-0.23094010767585,-0.5,-2.77555756156289E-17));
#6130=CARTESIAN_POINT('',(-0.23094010767585,-0.5,-2.82820063659975E-17));
#6131=CARTESIAN_POINT('',(-0.115470053837925,-0.5,-0.2));
#6132=CARTESIAN_POINT('',(-0.23094010767585,-0.8,-2.77555756156289E-17));
#6133=CARTESIAN_POINT('',(-0.23094010767585,-0.5,-2.82820063659975E-17));
#6134=CARTESIAN_POINT('',(-0.115470053837925,-0.8,-0.2));
#6135=CARTESIAN_POINT('Origin',(-0.115470053837925,-0.5,0.2));
#6136=CARTESIAN_POINT('',(-0.115470053837925,-0.5,0.2));
#6137=CARTESIAN_POINT('',(-0.23094010767585,-0.5,-2.82820063659975E-17));
#6138=CARTESIAN_POINT('',(-0.115470053837925,-0.8,0.2));
#6139=CARTESIAN_POINT('',(-0.115470053837925,-0.5,0.2));
#6140=CARTESIAN_POINT('',(-0.23094010767585,-0.8,-2.82820063659975E-17));
#6141=CARTESIAN_POINT('Origin',(0.115470053837925,-0.5,0.2));
#6142=CARTESIAN_POINT('',(0.115470053837925,-0.5,0.2));
#6143=CARTESIAN_POINT('',(-0.115470053837925,-0.5,0.2));
#6144=CARTESIAN_POINT('',(0.115470053837925,-0.8,0.2));
#6145=CARTESIAN_POINT('',(0.115470053837925,-0.5,0.2));
#6146=CARTESIAN_POINT('',(-0.115470053837925,-0.8,0.2));
#6147=CARTESIAN_POINT('Origin',(0.23094010767585,-0.5,0.));
#6148=CARTESIAN_POINT('',(0.115470053837925,-0.5,0.2));
#6149=CARTESIAN_POINT('',(0.115470053837925,-0.8,0.2));
#6150=CARTESIAN_POINT('Origin',(0.,-0.5,0.));
#6151=CARTESIAN_POINT('Origin',(0.,-0.8,0.));
#6152=CARTESIAN_POINT('Origin',(0.,-1.4,0.));
#6153=CARTESIAN_POINT('',(-0.24505,-1.4,3.00099698131059E-17));
#6154=CARTESIAN_POINT('Origin',(0.,-1.4,0.));
#6155=CARTESIAN_POINT('Origin',(0.375,0.5,0.));
#6156=CARTESIAN_POINT('',(-0.375,0.5,-4.59242549680257E-17));
#6157=CARTESIAN_POINT('Origin',(0.,0.5,0.));
#6158=CARTESIAN_POINT('Origin',(0.,0.475,0.));
#6159=CARTESIAN_POINT('',(-0.425,0.45,-5.20474889637625E-17));
#6160=CARTESIAN_POINT('Origin',(0.,0.45,0.));
#6161=CARTESIAN_POINT('',(-0.4,0.475,-4.89858719658941E-17));
#6162=CARTESIAN_POINT('Origin',(0.,0.24,0.));
#6163=CARTESIAN_POINT('',(-0.425,0.0299999999999998,-5.20474889637625E-17));
#6164=CARTESIAN_POINT('Origin',(0.,0.0299999999999998,0.));
#6165=CARTESIAN_POINT('',(-0.425,0.24,-5.20474889637625E-17));
#6166=CARTESIAN_POINT('Origin',(0.,0.0150000000000001,0.));
#6167=CARTESIAN_POINT('',(-0.395,4.85722573273506E-17,-4.83735485663204E-17));
#6168=CARTESIAN_POINT('Origin',(0.,0.,0.));
#6169=CARTESIAN_POINT('',(-0.41,0.0150000000000001,-5.02105187650415E-17));
#6170=CARTESIAN_POINT('Origin',(0.27,0.,0.));
#6171=CARTESIAN_POINT('',(-0.27,0.,-3.30654635769785E-17));
#6172=CARTESIAN_POINT('Origin',(0.,0.,0.));
#6173=CARTESIAN_POINT('Origin',(0.,-0.02,0.));
#6174=CARTESIAN_POINT('',(-0.24505,-0.0498999999999999,3.00099698131059E-17));
#6175=CARTESIAN_POINT('Origin',(0.,-0.0498999999999999,0.));
#6176=CARTESIAN_POINT('',(-0.26,-0.02,-3.18408167778312E-17));
#6177=CARTESIAN_POINT('Origin',(0.,-0.995,0.));
#6178=CARTESIAN_POINT('',(-0.24505,-0.995,-3.00099698131059E-17));
#6179=CARTESIAN_POINT('',(0.,0.,0.));
#6180=CARTESIAN_POINT('',(0.,0.,0.));
#6181=CARTESIAN_POINT('Origin',(20.,-1.9,16.));
#6182=CARTESIAN_POINT('',(19.725,-1.8,16.));
#6183=CARTESIAN_POINT('Origin',(20.,-1.8,16.));
#6184=CARTESIAN_POINT('',(19.725,-1.4,16.));
#6185=CARTESIAN_POINT('',(19.725,-1.9,16.));
#6186=CARTESIAN_POINT('Origin',(20.,-1.4,16.));
#6187=CARTESIAN_POINT('Origin',(4.5,-1.9,24.));
#6188=CARTESIAN_POINT('',(4.275,-1.8,24.));
#6189=CARTESIAN_POINT('Origin',(4.5,-1.8,24.));
#6190=CARTESIAN_POINT('',(4.275,-1.4,24.));
#6191=CARTESIAN_POINT('',(4.275,-1.9,24.));
#6192=CARTESIAN_POINT('Origin',(4.5,-1.4,24.));
#6193=CARTESIAN_POINT('Origin',(4.5,-1.9,7.2));
#6194=CARTESIAN_POINT('',(4.275,-1.8,7.2));
#6195=CARTESIAN_POINT('Origin',(4.5,-1.8,7.2));
#6196=CARTESIAN_POINT('',(4.275,-1.4,7.2));
#6197=CARTESIAN_POINT('',(4.275,-1.9,7.2));
#6198=CARTESIAN_POINT('Origin',(4.5,-1.4,7.2));
#6199=CARTESIAN_POINT('Origin',(4.5,-1.9,6.));
#6200=CARTESIAN_POINT('',(4.275,-1.8,6.));
#6201=CARTESIAN_POINT('Origin',(4.5,-1.8,6.));
#6202=CARTESIAN_POINT('',(4.275,-1.4,6.));
#6203=CARTESIAN_POINT('',(4.275,-1.9,6.));
#6204=CARTESIAN_POINT('Origin',(4.5,-1.4,6.));
#6205=CARTESIAN_POINT('Origin',(4.5,-1.9,25.2));
#6206=CARTESIAN_POINT('',(4.275,-1.8,25.2));
#6207=CARTESIAN_POINT('Origin',(4.5,-1.8,25.2));
#6208=CARTESIAN_POINT('',(4.275,-1.4,25.2));
#6209=CARTESIAN_POINT('',(4.275,-1.9,25.2));
#6210=CARTESIAN_POINT('Origin',(4.5,-1.4,25.2));
#6211=CARTESIAN_POINT('Origin',(20.5,-1.4,3.));
#6212=CARTESIAN_POINT('',(20.5,-1.4,3.));
#6213=CARTESIAN_POINT('',(4.,-1.4,3.));
#6214=CARTESIAN_POINT('',(20.5,-1.4,3.));
#6215=CARTESIAN_POINT('',(4.,-1.4,29.));
#6216=CARTESIAN_POINT('',(4.,-1.4,3.));
#6217=CARTESIAN_POINT('',(20.5,-1.4,29.));
#6218=CARTESIAN_POINT('',(20.5,-1.4,29.));
#6219=CARTESIAN_POINT('',(20.5,-1.4,3.));
#6220=CARTESIAN_POINT('Origin',(20.5,-1.8,3.));
#6221=CARTESIAN_POINT('',(20.5,-1.8,3.));
#6222=CARTESIAN_POINT('',(20.5,-1.8,3.));
#6223=CARTESIAN_POINT('',(20.5,-1.8,29.));
#6224=CARTESIAN_POINT('',(20.5,-1.8,29.));
#6225=CARTESIAN_POINT('',(20.5,-1.8,3.));
#6226=CARTESIAN_POINT('Origin',(4.,-1.8,3.));
#6227=CARTESIAN_POINT('',(4.,-1.8,3.));
#6228=CARTESIAN_POINT('',(4.,-1.8,3.));
#6229=CARTESIAN_POINT('',(4.,-1.8,29.));
#6230=CARTESIAN_POINT('',(4.,-1.8,29.));
#6231=CARTESIAN_POINT('',(4.,-1.8,3.));
#6232=CARTESIAN_POINT('Origin',(4.,-1.4,3.));
#6233=CARTESIAN_POINT('',(4.,-1.4,3.));
#6234=CARTESIAN_POINT('',(4.,-1.4,29.));
#6235=CARTESIAN_POINT('Origin',(12.25,-1.6,29.));
#6236=CARTESIAN_POINT('Origin',(12.25,-1.6,3.));
#6237=CARTESIAN_POINT('',(0.,0.,0.));
#6238=CARTESIAN_POINT('Origin',(4.5,-2.3,6.));
#6239=CARTESIAN_POINT('',(4.275,-2.2,6.));
#6240=CARTESIAN_POINT('Origin',(4.5,-2.2,6.));
#6241=CARTESIAN_POINT('',(4.275,-1.8,6.));
#6242=CARTESIAN_POINT('',(4.275,-2.3,6.));
#6243=CARTESIAN_POINT('Origin',(4.5,-1.8,6.));
#6244=CARTESIAN_POINT('Origin',(4.5,-2.3,7.2));
#6245=CARTESIAN_POINT('',(4.275,-2.2,7.2));
#6246=CARTESIAN_POINT('Origin',(4.5,-2.2,7.2));
#6247=CARTESIAN_POINT('',(4.275,-1.8,7.2));
#6248=CARTESIAN_POINT('',(4.275,-2.3,7.2));
#6249=CARTESIAN_POINT('Origin',(4.5,-1.8,7.2));
#6250=CARTESIAN_POINT('Origin',(2.,-1.8,6.));
#6251=CARTESIAN_POINT('',(1.69,-1.8,6.02));
#6252=CARTESIAN_POINT('Origin',(2.,-1.8,6.02));
#6253=CARTESIAN_POINT('',(1.69,-1.8,7.18));
#6254=CARTESIAN_POINT('',(1.69,-1.8,6.));
#6255=CARTESIAN_POINT('Origin',(2.,-1.8,7.18));
#6256=CARTESIAN_POINT('Origin',(2.8,-2.2,5.5));
#6257=CARTESIAN_POINT('',(2.8,-2.2,7.18));
#6258=CARTESIAN_POINT('',(2.8,-1.8,7.18));
#6259=CARTESIAN_POINT('',(2.8,-2.,7.18));
#6260=CARTESIAN_POINT('',(2.8,-2.2,7.7));
#6261=CARTESIAN_POINT('',(2.8,-2.2,7.7));
#6262=CARTESIAN_POINT('',(2.8,-1.8,7.7));
#6263=CARTESIAN_POINT('',(2.8,-2.2,7.7));
#6264=CARTESIAN_POINT('',(2.8,-1.8,7.7));
#6265=CARTESIAN_POINT('Origin',(2.8,-2.2,5.5));
#6266=CARTESIAN_POINT('',(2.8,-1.8,6.02));
#6267=CARTESIAN_POINT('',(2.8,-2.2,6.02));
#6268=CARTESIAN_POINT('',(2.8,-2.,6.02));
#6269=CARTESIAN_POINT('',(2.8,-1.8,5.5));
#6270=CARTESIAN_POINT('',(2.8,-1.8,7.7));
#6271=CARTESIAN_POINT('',(2.8,-2.2,5.5));
#6272=CARTESIAN_POINT('',(2.8,-2.2,5.5));
#6273=CARTESIAN_POINT('',(2.8,-2.2,7.7));
#6274=CARTESIAN_POINT('Origin',(5.5,-2.2,5.5));
#6275=CARTESIAN_POINT('',(5.5,-2.2,5.5));
#6276=CARTESIAN_POINT('',(2.8,-2.2,5.5));
#6277=CARTESIAN_POINT('',(5.5,-1.8,5.5));
#6278=CARTESIAN_POINT('',(2.8,-1.8,5.5));
#6279=CARTESIAN_POINT('',(5.5,-2.2,5.5));
#6280=CARTESIAN_POINT('Origin',(5.5,-2.2,7.7));
#6281=CARTESIAN_POINT('',(5.5,-2.2,7.7));
#6282=CARTESIAN_POINT('',(5.5,-2.2,5.5));
#6283=CARTESIAN_POINT('',(5.5,-1.8,7.7));
#6284=CARTESIAN_POINT('',(5.5,-1.8,5.5));
#6285=CARTESIAN_POINT('',(5.5,-2.2,7.7));
#6286=CARTESIAN_POINT('Origin',(2.8,-2.2,7.7));
#6287=CARTESIAN_POINT('',(5.5,-2.2,7.7));
#6288=CARTESIAN_POINT('',(5.5,-1.8,7.7));
#6289=CARTESIAN_POINT('Origin',(2.,-1.8,6.02));
#6290=CARTESIAN_POINT('',(2.44721359549996,-2.2,6.02));
#6291=CARTESIAN_POINT('',(2.,-2.2,6.02));
#6292=CARTESIAN_POINT('',(2.6,-1.8,6.02));
#6293=CARTESIAN_POINT('Origin',(2.,-1.8,6.02));
#6294=CARTESIAN_POINT('',(2.,-1.8,6.02));
#6295=CARTESIAN_POINT('Origin',(2.5,-2.2,6.6));
#6296=CARTESIAN_POINT('',(2.44721359549996,-2.2,7.18));
#6297=CARTESIAN_POINT('',(3.,-2.2,7.18));
#6298=CARTESIAN_POINT('',(2.44721359549996,-2.2,6.02));
#6299=CARTESIAN_POINT('Origin',(2.5,-1.8,6.6));
#6300=CARTESIAN_POINT('',(2.6,-1.8,7.18));
#6301=CARTESIAN_POINT('',(2.6,-1.8,6.02));
#6302=CARTESIAN_POINT('',(3.,-1.8,7.18));
#6303=CARTESIAN_POINT('Origin',(2.,-1.8,6.02));
#6304=CARTESIAN_POINT('Origin',(2.,-1.8,7.18));
#6305=CARTESIAN_POINT('Origin',(2.,-1.8,7.18));
#6306=CARTESIAN_POINT('',(0.,0.,0.));
#6307=CARTESIAN_POINT('Origin',(0.3,0.4,0.));
#6308=CARTESIAN_POINT('',(-0.3,0.4,-3.67394039744206E-17));
#6309=CARTESIAN_POINT('Origin',(0.,0.4,0.));
#6310=CARTESIAN_POINT('Origin',(0.,0.375,0.));
#6311=CARTESIAN_POINT('',(-0.35,0.35,-4.28626379701573E-17));
#6312=CARTESIAN_POINT('Origin',(0.,0.35,0.));
#6313=CARTESIAN_POINT('',(-0.325,0.375,-3.9801020972289E-17));
#6314=CARTESIAN_POINT('Origin',(0.,0.19,0.));
#6315=CARTESIAN_POINT('',(-0.35,0.03,-4.28626379701574E-17));
#6316=CARTESIAN_POINT('Origin',(0.,0.03,0.));
#6317=CARTESIAN_POINT('',(-0.35,0.19,-4.28626379701574E-17));
#6318=CARTESIAN_POINT('Origin',(0.,0.0149999999999999,0.));
#6319=CARTESIAN_POINT('',(-0.32,-3.29597460435593E-17,-3.91886975727153E-17));
#6320=CARTESIAN_POINT('Origin',(0.,0.,0.));
#6321=CARTESIAN_POINT('',(-0.335,0.0149999999999999,-4.10256677714363E-17));
#6322=CARTESIAN_POINT('Origin',(0.22,0.,0.));
#6323=CARTESIAN_POINT('',(-0.22,-6.93889390390723E-18,-2.69422295812418E-17));
#6324=CARTESIAN_POINT('Origin',(0.,0.,0.));
#6325=CARTESIAN_POINT('Origin',(0.,-0.02,0.));
#6326=CARTESIAN_POINT('',(-0.1954,-0.0492,2.39295984553393E-17));
#6327=CARTESIAN_POINT('Origin',(0.,-0.0492,0.));
#6328=CARTESIAN_POINT('',(-0.21,-0.02,-2.57175827820944E-17));
#6329=CARTESIAN_POINT('Origin',(0.,-0.8,0.));
#6330=CARTESIAN_POINT('',(-0.1954,-1.5646,2.39295984553393E-17));
#6331=CARTESIAN_POINT('Origin',(0.,-1.5646,0.));
#6332=CARTESIAN_POINT('',(-0.1954,-0.8,-2.39295984553393E-17));
#6333=CARTESIAN_POINT('Origin',(0.,-1.58,0.));
#6334=CARTESIAN_POINT('',(-0.16,-1.6,-1.95943487863577E-17));
#6335=CARTESIAN_POINT('Origin',(0.,-1.6,0.));
#6336=CARTESIAN_POINT('',(-0.18,-1.58,-2.20436423846524E-17));
#6337=CARTESIAN_POINT('Origin',(0.,-1.6,0.));
#6338=CARTESIAN_POINT('Origin',(0.0866025403784439,-0.4,-0.15));
#6339=CARTESIAN_POINT('',(0.173205080756888,-0.4,0.));
#6340=CARTESIAN_POINT('',(0.0866025403784439,-0.4,-0.15));
#6341=CARTESIAN_POINT('',(0.173205080756888,-0.4,0.));
#6342=CARTESIAN_POINT('',(0.0866025403784439,-0.64,-0.15));
#6343=CARTESIAN_POINT('',(0.0866025403784439,-0.4,-0.15));
#6344=CARTESIAN_POINT('',(0.173205080756888,-0.64,0.));
#6345=CARTESIAN_POINT('',(0.173205080756888,-0.64,0.));
#6346=CARTESIAN_POINT('',(0.173205080756888,-0.4,0.));
#6347=CARTESIAN_POINT('Origin',(-0.0866025403784438,-0.4,-0.15));
#6348=CARTESIAN_POINT('',(-0.0866025403784438,-0.4,-0.15));
#6349=CARTESIAN_POINT('',(0.0866025403784439,-0.4,-0.15));
#6350=CARTESIAN_POINT('',(-0.0866025403784438,-0.64,-0.15));
#6351=CARTESIAN_POINT('',(-0.0866025403784438,-0.4,-0.15));
#6352=CARTESIAN_POINT('',(0.0866025403784439,-0.64,-0.15));
#6353=CARTESIAN_POINT('Origin',(-0.173205080756888,-0.4,-2.77555756156289E-17));
#6354=CARTESIAN_POINT('',(-0.173205080756888,-0.4,-2.12115047744981E-17));
#6355=CARTESIAN_POINT('',(-0.0866025403784438,-0.4,-0.15));
#6356=CARTESIAN_POINT('',(-0.173205080756888,-0.64,-2.77555756156289E-17));
#6357=CARTESIAN_POINT('',(-0.173205080756888,-0.4,-2.12115047744981E-17));
#6358=CARTESIAN_POINT('',(-0.0866025403784438,-0.64,-0.15));
#6359=CARTESIAN_POINT('Origin',(-0.0866025403784439,-0.4,0.15));
#6360=CARTESIAN_POINT('',(-0.0866025403784439,-0.4,0.15));
#6361=CARTESIAN_POINT('',(-0.173205080756888,-0.4,-2.12115047744981E-17));
#6362=CARTESIAN_POINT('',(-0.0866025403784439,-0.64,0.15));
#6363=CARTESIAN_POINT('',(-0.0866025403784439,-0.4,0.15));
#6364=CARTESIAN_POINT('',(-0.173205080756888,-0.64,-2.12115047744981E-17));
#6365=CARTESIAN_POINT('Origin',(0.0866025403784439,-0.4,0.15));
#6366=CARTESIAN_POINT('',(0.0866025403784439,-0.4,0.15));
#6367=CARTESIAN_POINT('',(-0.0866025403784439,-0.4,0.15));
#6368=CARTESIAN_POINT('',(0.0866025403784439,-0.64,0.15));
#6369=CARTESIAN_POINT('',(0.0866025403784439,-0.4,0.15));
#6370=CARTESIAN_POINT('',(-0.0866025403784439,-0.64,0.15));
#6371=CARTESIAN_POINT('Origin',(0.173205080756888,-0.4,0.));
#6372=CARTESIAN_POINT('',(0.0866025403784439,-0.4,0.15));
#6373=CARTESIAN_POINT('',(0.0866025403784439,-0.64,0.15));
#6374=CARTESIAN_POINT('Origin',(0.,-0.4,-2.77555756156289E-17));
#6375=CARTESIAN_POINT('Origin',(0.,-0.64,-2.77555756156289E-17));
#6376=CARTESIAN_POINT('',(0.,0.,0.));
#6377=CARTESIAN_POINT('Origin',(0.,0.0495496978733727,0.));
#6378=CARTESIAN_POINT('',(-0.202072594216369,0.0413643688277828,0.35));
#6379=CARTESIAN_POINT('',(0.202072594216369,0.0413643688277828,0.35));
#6380=CARTESIAN_POINT('Ctrl Pts',(-0.202072594216369,0.0413643688277828,
0.35));
#6381=CARTESIAN_POINT('Ctrl Pts',(-1.66533453693773E-16,-0.0169689645055507,
0.35));
#6382=CARTESIAN_POINT('Ctrl Pts',(0.202072594216369,0.0413643688277828,
0.35));
#6383=CARTESIAN_POINT('',(-0.404145188432738,0.0413643688277828,-4.94935111404956E-17));
#6384=CARTESIAN_POINT('Ctrl Pts',(-0.404145188432738,0.0413643688277828,
-4.94935111404956E-17));
#6385=CARTESIAN_POINT('Ctrl Pts',(-0.303108891324553,-0.0169689645055504,
0.175));
#6386=CARTESIAN_POINT('Ctrl Pts',(-0.202072594216369,0.0413643688277828,
0.35));
#6387=CARTESIAN_POINT('',(-0.3325,0.,-4.07195060716495E-17));
#6388=CARTESIAN_POINT('',(-0.418322594216369,0.0495496978733727,-5.12297426018093E-17));
#6389=CARTESIAN_POINT('Origin',(0.,0.,0.));
#6390=CARTESIAN_POINT('',(-0.202072594216369,0.0413643688277828,-0.35));
#6391=CARTESIAN_POINT('Ctrl Pts',(-0.202072594216369,0.0413643688277828,
-0.35));
#6392=CARTESIAN_POINT('Ctrl Pts',(-0.303108891324553,-0.0169689645055505,
-0.175));
#6393=CARTESIAN_POINT('Ctrl Pts',(-0.404145188432738,0.0413643688277828,
-4.94935111404956E-17));
#6394=CARTESIAN_POINT('',(0.202072594216369,0.0413643688277828,-0.35));
#6395=CARTESIAN_POINT('Ctrl Pts',(0.202072594216369,0.0413643688277828,
-0.35));
#6396=CARTESIAN_POINT('Ctrl Pts',(-2.77555756156289E-17,-0.0169689645055504,
-0.35));
#6397=CARTESIAN_POINT('Ctrl Pts',(-0.202072594216369,0.0413643688277828,
-0.35));
#6398=CARTESIAN_POINT('',(0.404145188432738,0.0413643688277828,0.));
#6399=CARTESIAN_POINT('Ctrl Pts',(0.404145188432738,0.0413643688277828,
0.));
#6400=CARTESIAN_POINT('Ctrl Pts',(0.303108891324553,-0.0169689645055505,
-0.175));
#6401=CARTESIAN_POINT('Ctrl Pts',(0.202072594216369,0.0413643688277828,
-0.35));
#6402=CARTESIAN_POINT('Ctrl Pts',(0.202072594216369,0.0413643688277828,
0.35));
#6403=CARTESIAN_POINT('Ctrl Pts',(0.303108891324554,-0.0169689645055505,
0.175));
#6404=CARTESIAN_POINT('Ctrl Pts',(0.404145188432738,0.0413643688277828,
0.));
#6405=CARTESIAN_POINT('Origin',(0.,0.270450302126627,0.));
#6406=CARTESIAN_POINT('',(-0.3325,0.32,-4.07195060716495E-17));
#6407=CARTESIAN_POINT('Origin',(0.,0.32,0.));
#6408=CARTESIAN_POINT('',(-0.404145188432738,0.278635631172217,-4.94935111404957E-17));
#6409=CARTESIAN_POINT('',(-0.418322594216369,0.270450302126627,-5.12297426018093E-17));
#6410=CARTESIAN_POINT('',(-0.202072594216369,0.278635631172217,0.35));
#6411=CARTESIAN_POINT('Ctrl Pts',(-0.202072594216369,0.278635631172217,
0.35));
#6412=CARTESIAN_POINT('Ctrl Pts',(-0.303108891324554,0.33696896450555,0.175));
#6413=CARTESIAN_POINT('Ctrl Pts',(-0.404145188432738,0.278635631172217,
-4.94935111404957E-17));
#6414=CARTESIAN_POINT('',(0.202072594216369,0.278635631172217,0.35));
#6415=CARTESIAN_POINT('Ctrl Pts',(0.202072594216369,0.278635631172217,0.35));
#6416=CARTESIAN_POINT('Ctrl Pts',(-1.38777878078145E-16,0.336968964505551,
0.35));
#6417=CARTESIAN_POINT('Ctrl Pts',(-0.202072594216369,0.278635631172217,
0.35));
#6418=CARTESIAN_POINT('',(0.404145188432738,0.278635631172217,0.));
#6419=CARTESIAN_POINT('Ctrl Pts',(0.404145188432738,0.278635631172217,0.));
#6420=CARTESIAN_POINT('Ctrl Pts',(0.303108891324553,0.336968964505551,0.175));
#6421=CARTESIAN_POINT('Ctrl Pts',(0.202072594216369,0.278635631172217,0.35));
#6422=CARTESIAN_POINT('',(0.202072594216369,0.278635631172217,-0.35));
#6423=CARTESIAN_POINT('Ctrl Pts',(0.202072594216369,0.278635631172217,-0.35));
#6424=CARTESIAN_POINT('Ctrl Pts',(0.303108891324554,0.336968964505551,-0.175));
#6425=CARTESIAN_POINT('Ctrl Pts',(0.404145188432738,0.278635631172217,0.));
#6426=CARTESIAN_POINT('',(-0.202072594216369,0.278635631172217,-0.35));
#6427=CARTESIAN_POINT('Ctrl Pts',(-0.202072594216369,0.278635631172217,
-0.35));
#6428=CARTESIAN_POINT('Ctrl Pts',(8.32667268468867E-17,0.33696896450555,
-0.35));
#6429=CARTESIAN_POINT('Ctrl Pts',(0.202072594216369,0.278635631172217,-0.35));
#6430=CARTESIAN_POINT('Ctrl Pts',(-0.404145188432738,0.278635631172217,
-4.94935111404957E-17));
#6431=CARTESIAN_POINT('Ctrl Pts',(-0.303108891324553,0.33696896450555,-0.175));
#6432=CARTESIAN_POINT('Ctrl Pts',(-0.202072594216369,0.278635631172217,
-0.35));
#6433=CARTESIAN_POINT('Origin',(0.202072594216369,0.,-0.35));
#6434=CARTESIAN_POINT('',(-0.202072594216369,0.,-0.35));
#6435=CARTESIAN_POINT('',(0.202072594216369,0.,-0.35));
#6436=CARTESIAN_POINT('Origin',(-0.202072594216369,0.,-0.35));
#6437=CARTESIAN_POINT('',(-0.404145188432738,0.,-4.94935111404957E-17));
#6438=CARTESIAN_POINT('Origin',(-0.404145188432738,0.,-4.94935111404957E-17));
#6439=CARTESIAN_POINT('',(-0.202072594216369,0.,0.35));
#6440=CARTESIAN_POINT('Origin',(0.,0.,0.));
#6441=CARTESIAN_POINT('',(-0.1666,0.32,2.04026156737949E-17));
#6442=CARTESIAN_POINT('Origin',(0.,0.32,0.));
#6443=CARTESIAN_POINT('',(-0.1666,0.,2.04026156737949E-17));
#6444=CARTESIAN_POINT('',(-0.1666,0.,2.04026156737949E-17));
#6445=CARTESIAN_POINT('Origin',(0.,0.,0.));
#6446=CARTESIAN_POINT('Origin',(-0.202072594216369,0.,0.35));
#6447=CARTESIAN_POINT('',(0.202072594216369,0.,0.35));
#6448=CARTESIAN_POINT('Origin',(0.404145188432738,0.,0.));
#6449=CARTESIAN_POINT('',(0.404145188432738,0.,0.));
#6450=CARTESIAN_POINT('Origin',(0.202072594216369,0.,0.35));
#6451=CARTESIAN_POINT('Origin',(0.,0.32,0.));
#6452=CARTESIAN_POINT('Origin',(0.,0.,0.));
#6453=CARTESIAN_POINT('',(0.,0.,0.));
#6454=CARTESIAN_POINT('Origin',(0.,0.09,0.));
#6455=CARTESIAN_POINT('',(-0.285,0.1,3.49024337756996E-17));
#6456=CARTESIAN_POINT('Origin',(0.,0.1,0.));
#6457=CARTESIAN_POINT('',(-0.265,0.08,-3.24531401774049E-17));
#6458=CARTESIAN_POINT('',(-0.275,0.09,3.36777869765522E-17));
#6459=CARTESIAN_POINT('Origin',(0.,0.08,0.));
#6460=CARTESIAN_POINT('Origin',(0.,0.,0.));
#6461=CARTESIAN_POINT('',(-0.265,0.,3.24531401774049E-17));
#6462=CARTESIAN_POINT('',(-0.265,0.,3.24531401774049E-17));
#6463=CARTESIAN_POINT('Origin',(0.,0.,0.));
#6464=CARTESIAN_POINT('Origin',(0.,0.1,0.));
#6465=CARTESIAN_POINT('',(-0.5,0.1,6.12323399573677E-17));
#6466=CARTESIAN_POINT('Origin',(0.,0.1,0.));
#6467=CARTESIAN_POINT('Origin',(0.,0.,0.));
#6468=CARTESIAN_POINT('',(-0.5,0.,6.12323399573677E-17));
#6469=CARTESIAN_POINT('',(-0.5,0.,6.12323399573677E-17));
#6470=CARTESIAN_POINT('Origin',(0.,0.,0.));
#6471=CARTESIAN_POINT('Origin',(0.,0.,0.));
#6472=CARTESIAN_POINT('',(0.,0.,0.));
#6473=CARTESIAN_POINT('',(0.,0.,0.));
#6474=CARTESIAN_POINT('',(0.,0.,1.));
#6475=CARTESIAN_POINT('',(22.,0.,1.));
#6476=CARTESIAN_POINT('',(0.,0.,18.));
#6477=CARTESIAN_POINT('',(2.,-1.8,7.86));
#6478=CARTESIAN_POINT('',(2.,-1.8,5.34));
#6479=CARTESIAN_POINT('',(2.,-1.8,7.7));
#6480=CARTESIAN_POINT('',(1.6,-1.8,5.16));
#6481=CARTESIAN_POINT('',(0.,-0.42,6.));
#6482=CARTESIAN_POINT('',(0.,-1.8,6.));
#6483=CARTESIAN_POINT('',(0.,-1.9,6.));
#6484=CARTESIAN_POINT('',(0.,-0.42,7.2));
#6485=CARTESIAN_POINT('',(0.,-1.8,7.2));
#6486=CARTESIAN_POINT('',(0.,-1.9,7.2));
#6487=CARTESIAN_POINT('',(2.,-1.8,25.86));
#6488=CARTESIAN_POINT('',(2.,-1.8,23.34));
#6489=CARTESIAN_POINT('',(2.,-1.8,25.7));
#6490=CARTESIAN_POINT('',(1.6,-1.8,23.16));
#6491=CARTESIAN_POINT('',(0.,-0.42,24.));
#6492=CARTESIAN_POINT('',(0.,-1.8,24.));
#6493=CARTESIAN_POINT('',(0.,-1.9,24.));
#6494=CARTESIAN_POINT('',(0.,-0.42,25.2));
#6495=CARTESIAN_POINT('',(0.,-1.8,25.2));
#6496=CARTESIAN_POINT('',(0.,-1.9,25.2));
#6497=CARTESIAN_POINT('',(22.,-0.42,15.));
#6498=CARTESIAN_POINT('',(22.,-1.8,15.));
#6499=CARTESIAN_POINT('',(22.,-1.9,15.));
#6500=CARTESIAN_POINT('',(22.,-0.42,17.));
#6501=CARTESIAN_POINT('',(22.,-1.8,17.));
#6502=CARTESIAN_POINT('',(22.,-1.9,17.));
#6503=CARTESIAN_POINT('',(0.,0.,0.));
#6504=CARTESIAN_POINT('Origin',(0.375,0.5,0.));
#6505=CARTESIAN_POINT('',(-0.375,0.5,-4.59242549680257E-17));
#6506=CARTESIAN_POINT('Origin',(0.,0.5,0.));
#6507=CARTESIAN_POINT('Origin',(0.,0.475,0.));
#6508=CARTESIAN_POINT('',(-0.425,0.45,-5.20474889637625E-17));
#6509=CARTESIAN_POINT('Origin',(0.,0.45,0.));
#6510=CARTESIAN_POINT('',(-0.4,0.475,-4.89858719658941E-17));
#6511=CARTESIAN_POINT('Origin',(0.,0.24,0.));
#6512=CARTESIAN_POINT('',(-0.425,0.0299999999999998,-5.20474889637625E-17));
#6513=CARTESIAN_POINT('Origin',(0.,0.0299999999999998,0.));
#6514=CARTESIAN_POINT('',(-0.425,0.24,-5.20474889637625E-17));
#6515=CARTESIAN_POINT('Origin',(0.,0.0150000000000001,0.));
#6516=CARTESIAN_POINT('',(-0.395,4.85722573273506E-17,-4.83735485663204E-17));
#6517=CARTESIAN_POINT('Origin',(0.,0.,0.));
#6518=CARTESIAN_POINT('',(-0.41,0.0150000000000001,-5.02105187650415E-17));
#6519=CARTESIAN_POINT('Origin',(0.27,0.,0.));
#6520=CARTESIAN_POINT('',(-0.27,0.,-3.30654635769785E-17));
#6521=CARTESIAN_POINT('Origin',(0.,0.,0.));
#6522=CARTESIAN_POINT('Origin',(0.,-0.02,0.));
#6523=CARTESIAN_POINT('',(-0.24505,-0.0498999999999999,3.00099698131059E-17));
#6524=CARTESIAN_POINT('Origin',(0.,-0.0498999999999999,0.));
#6525=CARTESIAN_POINT('',(-0.26,-0.02,-3.18408167778312E-17));
#6526=CARTESIAN_POINT('Origin',(0.,-0.995,0.));
#6527=CARTESIAN_POINT('',(-0.24505,-1.95495,3.00099698131059E-17));
#6528=CARTESIAN_POINT('Origin',(0.,-1.95495,0.));
#6529=CARTESIAN_POINT('',(-0.24505,-0.995,-3.00099698131059E-17));
#6530=CARTESIAN_POINT('Origin',(0.,-1.975,0.));
#6531=CARTESIAN_POINT('',(-0.2,-2.,-2.44929359829471E-17));
#6532=CARTESIAN_POINT('Origin',(0.,-2.,0.));
#6533=CARTESIAN_POINT('',(-0.225,-1.975,-2.75545529808154E-17));
#6534=CARTESIAN_POINT('Origin',(0.,-2.,0.));
#6535=CARTESIAN_POINT('Origin',(0.115470053837925,-0.5,-0.2));
#6536=CARTESIAN_POINT('',(0.23094010767585,-0.5,0.));
#6537=CARTESIAN_POINT('',(0.115470053837925,-0.5,-0.2));
#6538=CARTESIAN_POINT('',(0.23094010767585,-0.5,0.));
#6539=CARTESIAN_POINT('',(0.115470053837925,-0.8,-0.2));
#6540=CARTESIAN_POINT('',(0.115470053837925,-0.5,-0.2));
#6541=CARTESIAN_POINT('',(0.23094010767585,-0.8,0.));
#6542=CARTESIAN_POINT('',(0.23094010767585,-0.8,0.));
#6543=CARTESIAN_POINT('',(0.23094010767585,-0.5,0.));
#6544=CARTESIAN_POINT('Origin',(-0.115470053837925,-0.5,-0.2));
#6545=CARTESIAN_POINT('',(-0.115470053837925,-0.5,-0.2));
#6546=CARTESIAN_POINT('',(0.115470053837925,-0.5,-0.2));
#6547=CARTESIAN_POINT('',(-0.115470053837925,-0.8,-0.2));
#6548=CARTESIAN_POINT('',(-0.115470053837925,-0.5,-0.2));
#6549=CARTESIAN_POINT('',(0.115470053837925,-0.8,-0.2));
#6550=CARTESIAN_POINT('Origin',(-0.23094010767585,-0.5,-2.77555756156289E-17));
#6551=CARTESIAN_POINT('',(-0.23094010767585,-0.5,-2.82820063659975E-17));
#6552=CARTESIAN_POINT('',(-0.115470053837925,-0.5,-0.2));
#6553=CARTESIAN_POINT('',(-0.23094010767585,-0.8,-2.77555756156289E-17));
#6554=CARTESIAN_POINT('',(-0.23094010767585,-0.5,-2.82820063659975E-17));
#6555=CARTESIAN_POINT('',(-0.115470053837925,-0.8,-0.2));
#6556=CARTESIAN_POINT('Origin',(-0.115470053837925,-0.5,0.2));
#6557=CARTESIAN_POINT('',(-0.115470053837925,-0.5,0.2));
#6558=CARTESIAN_POINT('',(-0.23094010767585,-0.5,-2.82820063659975E-17));
#6559=CARTESIAN_POINT('',(-0.115470053837925,-0.8,0.2));
#6560=CARTESIAN_POINT('',(-0.115470053837925,-0.5,0.2));
#6561=CARTESIAN_POINT('',(-0.23094010767585,-0.8,-2.82820063659975E-17));
#6562=CARTESIAN_POINT('Origin',(0.115470053837925,-0.5,0.2));
#6563=CARTESIAN_POINT('',(0.115470053837925,-0.5,0.2));
#6564=CARTESIAN_POINT('',(-0.115470053837925,-0.5,0.2));
#6565=CARTESIAN_POINT('',(0.115470053837925,-0.8,0.2));
#6566=CARTESIAN_POINT('',(0.115470053837925,-0.5,0.2));
#6567=CARTESIAN_POINT('',(-0.115470053837925,-0.8,0.2));
#6568=CARTESIAN_POINT('Origin',(0.23094010767585,-0.5,0.));
#6569=CARTESIAN_POINT('',(0.115470053837925,-0.5,0.2));
#6570=CARTESIAN_POINT('',(0.115470053837925,-0.8,0.2));
#6571=CARTESIAN_POINT('Origin',(0.,-0.5,0.));
#6572=CARTESIAN_POINT('Origin',(0.,-0.8,0.));
#6573=CARTESIAN_POINT('',(0.,0.,0.));
#6574=CARTESIAN_POINT('Origin',(0.,0.0525042956467857,0.));
#6575=CARTESIAN_POINT('',(-0.230940107675851,0.0472735643746089,0.4));
#6576=CARTESIAN_POINT('',(0.23094010767585,0.0472735643746089,0.4));
#6577=CARTESIAN_POINT('Ctrl Pts',(-0.230940107675851,0.0472735643746089,
0.4));
#6578=CARTESIAN_POINT('Ctrl Pts',(1.11022302462516E-16,-0.0193931022920578,
0.4));
#6579=CARTESIAN_POINT('Ctrl Pts',(0.23094010767585,0.0472735643746089,0.4));
#6580=CARTESIAN_POINT('',(-0.461880215351701,0.0472735643746089,-5.6564012731995E-17));
#6581=CARTESIAN_POINT('Ctrl Pts',(-0.461880215351701,0.0472735643746089,
-5.6564012731995E-17));
#6582=CARTESIAN_POINT('Ctrl Pts',(-0.346410161513776,-0.0193931022920579,
0.2));
#6583=CARTESIAN_POINT('Ctrl Pts',(-0.230940107675851,0.0472735643746089,
0.4));
#6584=CARTESIAN_POINT('',(-0.38,-2.08166817117217E-17,-4.65365783675994E-17));
#6585=CARTESIAN_POINT('',(-0.47094010767585,0.0525042956467857,-5.7673529545534E-17));
#6586=CARTESIAN_POINT('Origin',(0.,0.,0.));
#6587=CARTESIAN_POINT('',(-0.23094010767585,0.0472735643746089,-0.4));
#6588=CARTESIAN_POINT('Ctrl Pts',(-0.23094010767585,0.0472735643746089,
-0.4));
#6589=CARTESIAN_POINT('Ctrl Pts',(-0.346410161513775,-0.0193931022920578,
-0.2));
#6590=CARTESIAN_POINT('Ctrl Pts',(-0.461880215351701,0.0472735643746089,
-5.6564012731995E-17));
#6591=CARTESIAN_POINT('',(0.23094010767585,0.0472735643746089,-0.4));
#6592=CARTESIAN_POINT('Ctrl Pts',(0.23094010767585,0.0472735643746089,-0.4));
#6593=CARTESIAN_POINT('Ctrl Pts',(0.,-0.0193931022920578,-0.4));
#6594=CARTESIAN_POINT('Ctrl Pts',(-0.23094010767585,0.0472735643746089,
-0.4));
#6595=CARTESIAN_POINT('',(0.461880215351701,0.0472735643746089,0.));
#6596=CARTESIAN_POINT('Ctrl Pts',(0.461880215351701,0.0472735643746089,
0.));
#6597=CARTESIAN_POINT('Ctrl Pts',(0.346410161513776,-0.019393102292058,
-0.2));
#6598=CARTESIAN_POINT('Ctrl Pts',(0.23094010767585,0.0472735643746089,-0.4));
#6599=CARTESIAN_POINT('Ctrl Pts',(0.23094010767585,0.0472735643746089,0.4));
#6600=CARTESIAN_POINT('Ctrl Pts',(0.346410161513776,-0.0193931022920577,
0.2));
#6601=CARTESIAN_POINT('Ctrl Pts',(0.461880215351701,0.0472735643746089,
0.));
#6602=CARTESIAN_POINT('Origin',(0.,0.417495704353214,0.));
#6603=CARTESIAN_POINT('',(-0.38,0.47,-4.65365783675994E-17));
#6604=CARTESIAN_POINT('Origin',(0.,0.47,0.));
#6605=CARTESIAN_POINT('',(-0.461880215351701,0.422726435625391,-5.6564012731995E-17));
#6606=CARTESIAN_POINT('',(-0.47094010767585,0.417495704353214,-5.7673529545534E-17));
#6607=CARTESIAN_POINT('',(-0.230940107675851,0.422726435625391,0.4));
#6608=CARTESIAN_POINT('Ctrl Pts',(-0.230940107675851,0.422726435625391,
0.4));
#6609=CARTESIAN_POINT('Ctrl Pts',(-0.346410161513776,0.489393102292058,
0.2));
#6610=CARTESIAN_POINT('Ctrl Pts',(-0.461880215351701,0.422726435625391,
-5.6564012731995E-17));
#6611=CARTESIAN_POINT('',(0.23094010767585,0.422726435625391,0.4));
#6612=CARTESIAN_POINT('Ctrl Pts',(0.23094010767585,0.422726435625391,0.4));
#6613=CARTESIAN_POINT('Ctrl Pts',(8.32667268468867E-17,0.489393102292058,
0.4));
#6614=CARTESIAN_POINT('Ctrl Pts',(-0.230940107675851,0.422726435625391,
0.4));
#6615=CARTESIAN_POINT('',(0.461880215351701,0.422726435625391,0.));
#6616=CARTESIAN_POINT('Ctrl Pts',(0.461880215351701,0.422726435625391,0.));
#6617=CARTESIAN_POINT('Ctrl Pts',(0.346410161513776,0.489393102292058,0.2));
#6618=CARTESIAN_POINT('Ctrl Pts',(0.23094010767585,0.422726435625391,0.4));
#6619=CARTESIAN_POINT('',(0.23094010767585,0.422726435625391,-0.4));
#6620=CARTESIAN_POINT('Ctrl Pts',(0.23094010767585,0.422726435625391,-0.4));
#6621=CARTESIAN_POINT('Ctrl Pts',(0.346410161513775,0.489393102292058,-0.2));
#6622=CARTESIAN_POINT('Ctrl Pts',(0.461880215351701,0.422726435625391,0.));
#6623=CARTESIAN_POINT('',(-0.23094010767585,0.422726435625391,-0.4));
#6624=CARTESIAN_POINT('Ctrl Pts',(-0.23094010767585,0.422726435625391,-0.4));
#6625=CARTESIAN_POINT('Ctrl Pts',(-5.55111512312578E-17,0.489393102292058,
-0.4));
#6626=CARTESIAN_POINT('Ctrl Pts',(0.23094010767585,0.422726435625391,-0.4));
#6627=CARTESIAN_POINT('Ctrl Pts',(-0.461880215351701,0.422726435625391,
-5.6564012731995E-17));
#6628=CARTESIAN_POINT('Ctrl Pts',(-0.346410161513776,0.489393102292058,
-0.2));
#6629=CARTESIAN_POINT('Ctrl Pts',(-0.23094010767585,0.422726435625391,-0.4));
#6630=CARTESIAN_POINT('Origin',(0.23094010767585,0.,-0.4));
#6631=CARTESIAN_POINT('',(-0.23094010767585,0.,-0.4));
#6632=CARTESIAN_POINT('',(0.23094010767585,0.,-0.4));
#6633=CARTESIAN_POINT('Origin',(-0.23094010767585,0.,-0.4));
#6634=CARTESIAN_POINT('',(-0.461880215351701,0.,-5.6564012731995E-17));
#6635=CARTESIAN_POINT('Origin',(-0.461880215351701,0.,-5.6564012731995E-17));
#6636=CARTESIAN_POINT('',(-0.230940107675851,0.,0.4));
#6637=CARTESIAN_POINT('Origin',(0.,0.,0.));
#6638=CARTESIAN_POINT('',(-0.2117,0.47,2.59257727379495E-17));
#6639=CARTESIAN_POINT('Origin',(0.,0.47,0.));
#6640=CARTESIAN_POINT('',(-0.2117,0.,2.59257727379495E-17));
#6641=CARTESIAN_POINT('',(-0.2117,0.,2.59257727379495E-17));
#6642=CARTESIAN_POINT('Origin',(0.,0.,0.));
#6643=CARTESIAN_POINT('Origin',(-0.230940107675851,0.,0.4));
#6644=CARTESIAN_POINT('',(0.23094010767585,0.,0.4));
#6645=CARTESIAN_POINT('Origin',(0.461880215351701,0.,0.));
#6646=CARTESIAN_POINT('',(0.461880215351701,0.,0.));
#6647=CARTESIAN_POINT('Origin',(0.23094010767585,0.,0.4));
#6648=CARTESIAN_POINT('Origin',(0.,0.47,0.));
#6649=CARTESIAN_POINT('Origin',(0.,0.,0.));
#6650=CARTESIAN_POINT('',(0.,0.,0.));
#6651=CARTESIAN_POINT('',(0.,0.,0.));
#6652=CARTESIAN_POINT('',(0.,0.,18.));
#6653=CARTESIAN_POINT('',(4.5,-2.2,6.));
#6654=CARTESIAN_POINT('',(4.5,-1.4,6.));
#6655=CARTESIAN_POINT('',(4.5,-2.2,7.2));
#6656=CARTESIAN_POINT('',(4.5,-1.4,7.2));
#6657=CARTESIAN_POINT('',(4.5,-2.2,24.));
#6658=CARTESIAN_POINT('',(4.5,-1.4,24.));
#6659=CARTESIAN_POINT('',(4.5,-2.2,25.2));
#6660=CARTESIAN_POINT('',(4.5,-1.4,25.2));
#6661=CARTESIAN_POINT('',(20.,-2.2,16.));
#6662=CARTESIAN_POINT('',(20.,-2.3,16.));
#6663=CARTESIAN_POINT('',(20.,-1.4,16.));
#6664=CARTESIAN_POINT('',(0.,0.,0.));
#6665=CARTESIAN_POINT('',(0.,0.,0.));
#6666=CARTESIAN_POINT('Origin',(20.,-2.3,16.));
#6667=CARTESIAN_POINT('',(19.725,-2.2,16.));
#6668=CARTESIAN_POINT('Origin',(20.,-2.2,16.));
#6669=CARTESIAN_POINT('',(19.725,-1.8,16.));
#6670=CARTESIAN_POINT('',(19.725,-2.3,16.));
#6671=CARTESIAN_POINT('Origin',(20.,-1.8,16.));
#6672=CARTESIAN_POINT('Origin',(23.5,-1.8,15.5));
#6673=CARTESIAN_POINT('',(23.5,-1.8,15.5));
#6674=CARTESIAN_POINT('',(19.,-1.8,15.5));
#6675=CARTESIAN_POINT('',(23.5,-1.8,15.5));
#6676=CARTESIAN_POINT('',(19.,-1.8,16.5));
#6677=CARTESIAN_POINT('',(19.,-1.8,15.5));
#6678=CARTESIAN_POINT('',(23.5,-1.8,16.5));
#6679=CARTESIAN_POINT('',(23.5,-1.8,16.5));
#6680=CARTESIAN_POINT('',(23.5,-1.8,15.5));
#6681=CARTESIAN_POINT('Origin',(23.5,-2.2,15.5));
#6682=CARTESIAN_POINT('',(23.5,-2.2,15.5));
#6683=CARTESIAN_POINT('',(23.5,-2.2,15.5));
#6684=CARTESIAN_POINT('',(23.5,-2.2,16.5));
#6685=CARTESIAN_POINT('',(23.5,-2.2,16.5));
#6686=CARTESIAN_POINT('',(23.5,-2.2,15.5));
#6687=CARTESIAN_POINT('Origin',(19.,-2.2,15.5));
#6688=CARTESIAN_POINT('',(19.,-2.2,15.5));
#6689=CARTESIAN_POINT('',(19.,-2.2,15.5));
#6690=CARTESIAN_POINT('',(19.,-2.2,16.5));
#6691=CARTESIAN_POINT('',(19.,-2.2,16.5));
#6692=CARTESIAN_POINT('',(19.,-2.2,15.5));
#6693=CARTESIAN_POINT('Origin',(19.,-1.8,15.5));
#6694=CARTESIAN_POINT('',(19.,-1.8,15.5));
#6695=CARTESIAN_POINT('',(19.,-1.8,16.5));
#6696=CARTESIAN_POINT('Origin',(21.25,-2.,16.5));
#6697=CARTESIAN_POINT('Origin',(21.25,-2.,15.5));
#6698=CARTESIAN_POINT('',(0.,0.,0.));
#6699=CARTESIAN_POINT('',(0.,0.,0.));
#6700=CARTESIAN_POINT('',(0.,0.,0.));
#6701=CARTESIAN_POINT('',(0.,0.,0.));
#6702=UNCERTAINTY_MEASURE_WITH_UNIT(LENGTH_MEASURE(0.001),#6744,
'DISTANCE_ACCURACY_VALUE',
'Maximum model space distance between geometric entities at asserted c
onnectivities');
#6703=UNCERTAINTY_MEASURE_WITH_UNIT(LENGTH_MEASURE(0.001),#6744,
'DISTANCE_ACCURACY_VALUE',
'Maximum model space distance between geometric entities at asserted c
onnectivities');
#6704=UNCERTAINTY_MEASURE_WITH_UNIT(LENGTH_MEASURE(0.001),#6744,
'DISTANCE_ACCURACY_VALUE',
'Maximum model space distance between geometric entities at asserted c
onnectivities');
#6705=UNCERTAINTY_MEASURE_WITH_UNIT(LENGTH_MEASURE(0.001),#6744,
'DISTANCE_ACCURACY_VALUE',
'Maximum model space distance between geometric entities at asserted c
onnectivities');
#6706=UNCERTAINTY_MEASURE_WITH_UNIT(LENGTH_MEASURE(0.001),#6744,
'DISTANCE_ACCURACY_VALUE',
'Maximum model space distance between geometric entities at asserted c
onnectivities');
#6707=UNCERTAINTY_MEASURE_WITH_UNIT(LENGTH_MEASURE(0.001),#6744,
'DISTANCE_ACCURACY_VALUE',
'Maximum model space distance between geometric entities at asserted c
onnectivities');
#6708=UNCERTAINTY_MEASURE_WITH_UNIT(LENGTH_MEASURE(0.001),#6744,
'DISTANCE_ACCURACY_VALUE',
'Maximum model space distance between geometric entities at asserted c
onnectivities');
#6709=UNCERTAINTY_MEASURE_WITH_UNIT(LENGTH_MEASURE(0.001),#6744,
'DISTANCE_ACCURACY_VALUE',
'Maximum model space distance between geometric entities at asserted c
onnectivities');
#6710=UNCERTAINTY_MEASURE_WITH_UNIT(LENGTH_MEASURE(0.001),#6744,
'DISTANCE_ACCURACY_VALUE',
'Maximum model space distance between geometric entities at asserted c
onnectivities');
#6711=UNCERTAINTY_MEASURE_WITH_UNIT(LENGTH_MEASURE(0.001),#6744,
'DISTANCE_ACCURACY_VALUE',
'Maximum model space distance between geometric entities at asserted c
onnectivities');
#6712=UNCERTAINTY_MEASURE_WITH_UNIT(LENGTH_MEASURE(0.001),#6744,
'DISTANCE_ACCURACY_VALUE',
'Maximum model space distance between geometric entities at asserted c
onnectivities');
#6713=UNCERTAINTY_MEASURE_WITH_UNIT(LENGTH_MEASURE(0.001),#6744,
'DISTANCE_ACCURACY_VALUE',
'Maximum model space distance between geometric entities at asserted c
onnectivities');
#6714=UNCERTAINTY_MEASURE_WITH_UNIT(LENGTH_MEASURE(0.001),#6744,
'DISTANCE_ACCURACY_VALUE',
'Maximum model space distance between geometric entities at asserted c
onnectivities');
#6715=UNCERTAINTY_MEASURE_WITH_UNIT(LENGTH_MEASURE(0.001),#6744,
'DISTANCE_ACCURACY_VALUE',
'Maximum model space distance between geometric entities at asserted c
onnectivities');
#6716=UNCERTAINTY_MEASURE_WITH_UNIT(LENGTH_MEASURE(0.001),#6744,
'DISTANCE_ACCURACY_VALUE',
'Maximum model space distance between geometric entities at asserted c
onnectivities');
#6717=UNCERTAINTY_MEASURE_WITH_UNIT(LENGTH_MEASURE(0.001),#6744,
'DISTANCE_ACCURACY_VALUE',
'Maximum model space distance between geometric entities at asserted c
onnectivities');
#6718=UNCERTAINTY_MEASURE_WITH_UNIT(LENGTH_MEASURE(0.001),#6744,
'DISTANCE_ACCURACY_VALUE',
'Maximum model space distance between geometric entities at asserted c
onnectivities');
#6719=UNCERTAINTY_MEASURE_WITH_UNIT(LENGTH_MEASURE(0.001),#6744,
'DISTANCE_ACCURACY_VALUE',
'Maximum model space distance between geometric entities at asserted c
onnectivities');
#6720=UNCERTAINTY_MEASURE_WITH_UNIT(LENGTH_MEASURE(0.001),#6744,
'DISTANCE_ACCURACY_VALUE',
'Maximum model space distance between geometric entities at asserted c
onnectivities');
#6721=UNCERTAINTY_MEASURE_WITH_UNIT(LENGTH_MEASURE(0.001),#6744,
'DISTANCE_ACCURACY_VALUE',
'Maximum model space distance between geometric entities at asserted c
onnectivities');
#6722=UNCERTAINTY_MEASURE_WITH_UNIT(LENGTH_MEASURE(0.001),#6744,
'DISTANCE_ACCURACY_VALUE',
'Maximum model space distance between geometric entities at asserted c
onnectivities');
#6723=(
GEOMETRIC_REPRESENTATION_CONTEXT(3)
GLOBAL_UNCERTAINTY_ASSIGNED_CONTEXT((#6702))
GLOBAL_UNIT_ASSIGNED_CONTEXT((#6744,#6746,#6747))
REPRESENTATION_CONTEXT('','3D')
);
#6724=(
GEOMETRIC_REPRESENTATION_CONTEXT(3)
GLOBAL_UNCERTAINTY_ASSIGNED_CONTEXT((#6703))
GLOBAL_UNIT_ASSIGNED_CONTEXT((#6744,#6746,#6747))
REPRESENTATION_CONTEXT('','3D')
);
#6725=(
GEOMETRIC_REPRESENTATION_CONTEXT(3)
GLOBAL_UNCERTAINTY_ASSIGNED_CONTEXT((#6704))
GLOBAL_UNIT_ASSIGNED_CONTEXT((#6744,#6746,#6747))
REPRESENTATION_CONTEXT('','3D')
);
#6726=(
GEOMETRIC_REPRESENTATION_CONTEXT(3)
GLOBAL_UNCERTAINTY_ASSIGNED_CONTEXT((#6705))
GLOBAL_UNIT_ASSIGNED_CONTEXT((#6744,#6746,#6747))
REPRESENTATION_CONTEXT('','3D')
);
#6727=(
GEOMETRIC_REPRESENTATION_CONTEXT(3)
GLOBAL_UNCERTAINTY_ASSIGNED_CONTEXT((#6706))
GLOBAL_UNIT_ASSIGNED_CONTEXT((#6744,#6746,#6747))
REPRESENTATION_CONTEXT('','3D')
);
#6728=(
GEOMETRIC_REPRESENTATION_CONTEXT(3)
GLOBAL_UNCERTAINTY_ASSIGNED_CONTEXT((#6707))
GLOBAL_UNIT_ASSIGNED_CONTEXT((#6744,#6746,#6747))
REPRESENTATION_CONTEXT('','3D')
);
#6729=(
GEOMETRIC_REPRESENTATION_CONTEXT(3)
GLOBAL_UNCERTAINTY_ASSIGNED_CONTEXT((#6708))
GLOBAL_UNIT_ASSIGNED_CONTEXT((#6744,#6746,#6747))
REPRESENTATION_CONTEXT('','3D')
);
#6730=(
GEOMETRIC_REPRESENTATION_CONTEXT(3)
GLOBAL_UNCERTAINTY_ASSIGNED_CONTEXT((#6709))
GLOBAL_UNIT_ASSIGNED_CONTEXT((#6744,#6746,#6747))
REPRESENTATION_CONTEXT('','3D')
);
#6731=(
GEOMETRIC_REPRESENTATION_CONTEXT(3)
GLOBAL_UNCERTAINTY_ASSIGNED_CONTEXT((#6710))
GLOBAL_UNIT_ASSIGNED_CONTEXT((#6744,#6746,#6747))
REPRESENTATION_CONTEXT('','3D')
);
#6732=(
GEOMETRIC_REPRESENTATION_CONTEXT(3)
GLOBAL_UNCERTAINTY_ASSIGNED_CONTEXT((#6711))
GLOBAL_UNIT_ASSIGNED_CONTEXT((#6744,#6746,#6747))
REPRESENTATION_CONTEXT('','3D')
);
#6733=(
GEOMETRIC_REPRESENTATION_CONTEXT(3)
GLOBAL_UNCERTAINTY_ASSIGNED_CONTEXT((#6712))
GLOBAL_UNIT_ASSIGNED_CONTEXT((#6744,#6746,#6747))
REPRESENTATION_CONTEXT('','3D')
);
#6734=(
GEOMETRIC_REPRESENTATION_CONTEXT(3)
GLOBAL_UNCERTAINTY_ASSIGNED_CONTEXT((#6713))
GLOBAL_UNIT_ASSIGNED_CONTEXT((#6744,#6746,#6747))
REPRESENTATION_CONTEXT('','3D')
);
#6735=(
GEOMETRIC_REPRESENTATION_CONTEXT(3)
GLOBAL_UNCERTAINTY_ASSIGNED_CONTEXT((#6714))
GLOBAL_UNIT_ASSIGNED_CONTEXT((#6744,#6746,#6747))
REPRESENTATION_CONTEXT('','3D')
);
#6736=(
GEOMETRIC_REPRESENTATION_CONTEXT(3)
GLOBAL_UNCERTAINTY_ASSIGNED_CONTEXT((#6715))
GLOBAL_UNIT_ASSIGNED_CONTEXT((#6744,#6746,#6747))
REPRESENTATION_CONTEXT('','3D')
);
#6737=(
GEOMETRIC_REPRESENTATION_CONTEXT(3)
GLOBAL_UNCERTAINTY_ASSIGNED_CONTEXT((#6716))
GLOBAL_UNIT_ASSIGNED_CONTEXT((#6744,#6746,#6747))
REPRESENTATION_CONTEXT('','3D')
);
#6738=(
GEOMETRIC_REPRESENTATION_CONTEXT(3)
GLOBAL_UNCERTAINTY_ASSIGNED_CONTEXT((#6717))
GLOBAL_UNIT_ASSIGNED_CONTEXT((#6744,#6746,#6747))
REPRESENTATION_CONTEXT('','3D')
);
#6739=(
GEOMETRIC_REPRESENTATION_CONTEXT(3)
GLOBAL_UNCERTAINTY_ASSIGNED_CONTEXT((#6718))
GLOBAL_UNIT_ASSIGNED_CONTEXT((#6744,#6746,#6747))
REPRESENTATION_CONTEXT('','3D')
);
#6740=(
GEOMETRIC_REPRESENTATION_CONTEXT(3)
GLOBAL_UNCERTAINTY_ASSIGNED_CONTEXT((#6719))
GLOBAL_UNIT_ASSIGNED_CONTEXT((#6744,#6746,#6747))
REPRESENTATION_CONTEXT('','3D')
);
#6741=(
GEOMETRIC_REPRESENTATION_CONTEXT(3)
GLOBAL_UNCERTAINTY_ASSIGNED_CONTEXT((#6720))
GLOBAL_UNIT_ASSIGNED_CONTEXT((#6744,#6746,#6747))
REPRESENTATION_CONTEXT('','3D')
);
#6742=(
GEOMETRIC_REPRESENTATION_CONTEXT(3)
GLOBAL_UNCERTAINTY_ASSIGNED_CONTEXT((#6721))
GLOBAL_UNIT_ASSIGNED_CONTEXT((#6744,#6746,#6747))
REPRESENTATION_CONTEXT('','3D')
);
#6743=(
GEOMETRIC_REPRESENTATION_CONTEXT(3)
GLOBAL_UNCERTAINTY_ASSIGNED_CONTEXT((#6722))
GLOBAL_UNIT_ASSIGNED_CONTEXT((#6744,#6746,#6747))
REPRESENTATION_CONTEXT('','3D')
);
#6744=(
LENGTH_UNIT()
NAMED_UNIT(*)
SI_UNIT(.CENTI.,.METRE.)
);
#6745=(
LENGTH_UNIT()
NAMED_UNIT(*)
SI_UNIT($,.METRE.)
);
#6746=(
NAMED_UNIT(*)
PLANE_ANGLE_UNIT()
SI_UNIT($,.RADIAN.)
);
#6747=(
NAMED_UNIT(*)
SI_UNIT($,.STERADIAN.)
SOLID_ANGLE_UNIT()
);
#6748=SHAPE_DEFINITION_REPRESENTATION(#6768,#6837);
#6749=SHAPE_DEFINITION_REPRESENTATION(#6769,#6838);
#6750=SHAPE_DEFINITION_REPRESENTATION(#6770,#6839);
#6751=SHAPE_DEFINITION_REPRESENTATION(#6771,#6840);
#6752=SHAPE_DEFINITION_REPRESENTATION(#6772,#6841);
#6753=SHAPE_DEFINITION_REPRESENTATION(#6773,#6842);
#6754=SHAPE_DEFINITION_REPRESENTATION(#6774,#6843);
#6755=SHAPE_DEFINITION_REPRESENTATION(#6775,#6844);
#6756=SHAPE_DEFINITION_REPRESENTATION(#6776,#6845);
#6757=SHAPE_DEFINITION_REPRESENTATION(#6777,#6846);
#6758=SHAPE_DEFINITION_REPRESENTATION(#6778,#6847);
#6759=SHAPE_DEFINITION_REPRESENTATION(#6779,#6848);
#6760=SHAPE_DEFINITION_REPRESENTATION(#6780,#6849);
#6761=SHAPE_DEFINITION_REPRESENTATION(#6781,#6850);
#6762=SHAPE_DEFINITION_REPRESENTATION(#6782,#6851);
#6763=SHAPE_DEFINITION_REPRESENTATION(#6783,#6852);
#6764=SHAPE_DEFINITION_REPRESENTATION(#6815,#6853);
#6765=SHAPE_DEFINITION_REPRESENTATION(#6816,#6854);
#6766=SHAPE_DEFINITION_REPRESENTATION(#6831,#6855);
#6767=SHAPE_DEFINITION_REPRESENTATION(#6832,#6856);
#6768=PRODUCT_DEFINITION_SHAPE('',$,#6858);
#6769=PRODUCT_DEFINITION_SHAPE('',$,#6859);
#6770=PRODUCT_DEFINITION_SHAPE('',$,#6860);
#6771=PRODUCT_DEFINITION_SHAPE('',$,#6861);
#6772=PRODUCT_DEFINITION_SHAPE('',$,#6862);
#6773=PRODUCT_DEFINITION_SHAPE('',$,#6863);
#6774=PRODUCT_DEFINITION_SHAPE('',$,#6864);
#6775=PRODUCT_DEFINITION_SHAPE('',$,#6865);
#6776=PRODUCT_DEFINITION_SHAPE('',$,#6866);
#6777=PRODUCT_DEFINITION_SHAPE('',$,#6867);
#6778=PRODUCT_DEFINITION_SHAPE('',$,#6868);
#6779=PRODUCT_DEFINITION_SHAPE('',$,#6869);
#6780=PRODUCT_DEFINITION_SHAPE('',$,#6870);
#6781=PRODUCT_DEFINITION_SHAPE('',$,#6871);
#6782=PRODUCT_DEFINITION_SHAPE('',$,#6872);
#6783=PRODUCT_DEFINITION_SHAPE('',$,#6873);
#6784=PRODUCT_DEFINITION_SHAPE($,$,#158);
#6785=PRODUCT_DEFINITION_SHAPE($,$,#159);
#6786=PRODUCT_DEFINITION_SHAPE($,$,#160);
#6787=PRODUCT_DEFINITION_SHAPE($,$,#161);
#6788=PRODUCT_DEFINITION_SHAPE($,$,#162);
#6789=PRODUCT_DEFINITION_SHAPE($,$,#163);
#6790=PRODUCT_DEFINITION_SHAPE($,$,#164);
#6791=PRODUCT_DEFINITION_SHAPE($,$,#165);
#6792=PRODUCT_DEFINITION_SHAPE($,$,#166);
#6793=PRODUCT_DEFINITION_SHAPE($,$,#167);
#6794=PRODUCT_DEFINITION_SHAPE($,$,#168);
#6795=PRODUCT_DEFINITION_SHAPE($,$,#169);
#6796=PRODUCT_DEFINITION_SHAPE($,$,#170);
#6797=PRODUCT_DEFINITION_SHAPE($,$,#171);
#6798=PRODUCT_DEFINITION_SHAPE($,$,#172);
#6799=PRODUCT_DEFINITION_SHAPE($,$,#173);
#6800=PRODUCT_DEFINITION_SHAPE($,$,#174);
#6801=PRODUCT_DEFINITION_SHAPE($,$,#175);
#6802=PRODUCT_DEFINITION_SHAPE($,$,#176);
#6803=PRODUCT_DEFINITION_SHAPE($,$,#177);
#6804=PRODUCT_DEFINITION_SHAPE($,$,#178);
#6805=PRODUCT_DEFINITION_SHAPE($,$,#179);
#6806=PRODUCT_DEFINITION_SHAPE($,$,#180);
#6807=PRODUCT_DEFINITION_SHAPE($,$,#181);
#6808=PRODUCT_DEFINITION_SHAPE($,$,#182);
#6809=PRODUCT_DEFINITION_SHAPE($,$,#183);
#6810=PRODUCT_DEFINITION_SHAPE($,$,#184);
#6811=PRODUCT_DEFINITION_SHAPE($,$,#185);
#6812=PRODUCT_DEFINITION_SHAPE($,$,#186);
#6813=PRODUCT_DEFINITION_SHAPE($,$,#187);
#6814=PRODUCT_DEFINITION_SHAPE($,$,#188);
#6815=PRODUCT_DEFINITION_SHAPE('',$,#6874);
#6816=PRODUCT_DEFINITION_SHAPE('',$,#6875);
#6817=PRODUCT_DEFINITION_SHAPE($,$,#189);
#6818=PRODUCT_DEFINITION_SHAPE($,$,#190);
#6819=PRODUCT_DEFINITION_SHAPE($,$,#191);
#6820=PRODUCT_DEFINITION_SHAPE($,$,#192);
#6821=PRODUCT_DEFINITION_SHAPE($,$,#193);
#6822=PRODUCT_DEFINITION_SHAPE($,$,#194);
#6823=PRODUCT_DEFINITION_SHAPE($,$,#195);
#6824=PRODUCT_DEFINITION_SHAPE($,$,#196);
#6825=PRODUCT_DEFINITION_SHAPE($,$,#197);
#6826=PRODUCT_DEFINITION_SHAPE($,$,#198);
#6827=PRODUCT_DEFINITION_SHAPE($,$,#199);
#6828=PRODUCT_DEFINITION_SHAPE($,$,#200);
#6829=PRODUCT_DEFINITION_SHAPE($,$,#201);
#6830=PRODUCT_DEFINITION_SHAPE($,$,#202);
#6831=PRODUCT_DEFINITION_SHAPE('',$,#6876);
#6832=PRODUCT_DEFINITION_SHAPE('',$,#6877);
#6833=PRODUCT_DEFINITION_SHAPE($,$,#203);
#6834=PRODUCT_DEFINITION_SHAPE($,$,#204);
#6835=PRODUCT_DEFINITION_SHAPE($,$,#205);
#6836=PRODUCT_DEFINITION_SHAPE($,$,#206);
#6837=SHAPE_REPRESENTATION('',(#3994,#4361,#4362,#4363),#6723);
#6838=SHAPE_REPRESENTATION('',(#3995,#4262,#4263,#4264,#4265,#4266,#4267,
#4268,#4269,#4270,#4271,#4272,#4273,#4274,#4275,#4276,#4277,#4278,#4279,
#4280,#4281,#4282,#4283,#4284,#4285,#4286,#4287,#4288,#4289,#4290,#4291,
#4292),#6724);
#6839=SHAPE_REPRESENTATION('',(#3996),#6725);
#6840=SHAPE_REPRESENTATION('',(#4009),#6726);
#6841=SHAPE_REPRESENTATION('',(#4059),#6727);
#6842=SHAPE_REPRESENTATION('',(#4088),#6728);
#6843=SHAPE_REPRESENTATION('',(#4103),#6729);
#6844=SHAPE_REPRESENTATION('',(#4112),#6730);
#6845=SHAPE_REPRESENTATION('',(#4123),#6731);
#6846=SHAPE_REPRESENTATION('',(#4140),#6732);
#6847=SHAPE_REPRESENTATION('',(#4164,#4335,#4336,#4337,#4338,#4339,#4340,
#4341,#4342,#4343,#4344,#4345,#4346,#4347,#4348),#6733);
#6848=SHAPE_REPRESENTATION('',(#4165),#6734);
#6849=SHAPE_REPRESENTATION('',(#4187),#6735);
#6850=SHAPE_REPRESENTATION('',(#4209),#6736);
#6851=SHAPE_REPRESENTATION('',(#4235),#6737);
#6852=SHAPE_REPRESENTATION('',(#4251),#6738);
#6853=SHAPE_REPRESENTATION('',(#4293),#6739);
#6854=SHAPE_REPRESENTATION('',(#4319),#6740);
#6855=SHAPE_REPRESENTATION('',(#4349,#4360),#6741);
#6856=SHAPE_REPRESENTATION('',(#4350),#6742);
#6857=PRODUCT_DEFINITION_CONTEXT('part definition',#6919,'design');
#6858=PRODUCT_DEFINITION('PAT-055','PAT-055',#6878,#6857);
#6859=PRODUCT_DEFINITION('Extrusion jambs and fixed hinge leaves',
'Extrusion jambs and fixed hinge leaves',#6879,#6857);
#6860=PRODUCT_DEFINITION('Latch strike plate','Latch strike plate',#6880,
#6857);
#6861=PRODUCT_DEFINITION('Slotted Extrusion - 20 x 20 x 300 mm',
'Slotted Extrusion - 20 x 20 x 300 mm',#6881,#6857);
#6862=PRODUCT_DEFINITION('Fixed hinge leaf','Fixed hinge leaf',#6882,#6857);
#6863=PRODUCT_DEFINITION('Clevis Pin - 6x30','Clevis Pin - 6x30',#6883,
#6857);
#6864=PRODUCT_DEFINITION('Flat Washer - M6','Flat Washer - M6',#6884,#6857);
#6865=PRODUCT_DEFINITION('Split Pin - 1.6x16','Split Pin - 1.6x16',#6885,
#6857);
#6866=PRODUCT_DEFINITION('Slot Nut - M5 for 20 mm Extrusion',
'Slot Nut - M5 for 20 mm Extrusion',#6886,#6857);
#6867=PRODUCT_DEFINITION('M5x14 Cap Screw','M5x14 Cap Screw',#6887,#6857);
#6868=PRODUCT_DEFINITION('Panel and moving hinge leaves',
'Panel and moving hinge leaves',#6888,#6857);
#6869=PRODUCT_DEFINITION('Door panel','Door panel',#6889,#6857);
#6870=PRODUCT_DEFINITION('Moving hinge leaf','Moving hinge leaf',#6890,
#6857);
#6871=PRODUCT_DEFINITION('Cap Screw - M4x16','Cap Screw - M4x16',#6891,
#6857);
#6872=PRODUCT_DEFINITION('Hex Nut - M4','Hex Nut - M4',#6892,#6857);
#6873=PRODUCT_DEFINITION('Flat Washer - M5','Flat Washer - M5',#6893,#6857);
#6874=PRODUCT_DEFINITION('Cap Screw - M5x20','Cap Screw - M5x20',#6894,
#6857);
#6875=PRODUCT_DEFINITION('Hex Nut - M5','Hex Nut - M5',#6895,#6857);
#6876=PRODUCT_DEFINITION('Turn-button latch','Turn-button latch',#6896,
#6857);
#6877=PRODUCT_DEFINITION('Turn-button latch (1)','Turn-button latch (1)',
#6897,#6857);
#6878=PRODUCT_DEFINITION_FORMATION('',$,#6921);
#6879=PRODUCT_DEFINITION_FORMATION('',$,#6922);
#6880=PRODUCT_DEFINITION_FORMATION('',$,#6923);
#6881=PRODUCT_DEFINITION_FORMATION('',$,#6924);
#6882=PRODUCT_DEFINITION_FORMATION('',$,#6925);
#6883=PRODUCT_DEFINITION_FORMATION('',$,#6926);
#6884=PRODUCT_DEFINITION_FORMATION('',$,#6927);
#6885=PRODUCT_DEFINITION_FORMATION('',$,#6928);
#6886=PRODUCT_DEFINITION_FORMATION('',$,#6929);
#6887=PRODUCT_DEFINITION_FORMATION('',$,#6930);
#6888=PRODUCT_DEFINITION_FORMATION('',$,#6931);
#6889=PRODUCT_DEFINITION_FORMATION('',$,#6932);
#6890=PRODUCT_DEFINITION_FORMATION('',$,#6933);
#6891=PRODUCT_DEFINITION_FORMATION('',$,#6934);
#6892=PRODUCT_DEFINITION_FORMATION('',$,#6935);
#6893=PRODUCT_DEFINITION_FORMATION('',$,#6936);
#6894=PRODUCT_DEFINITION_FORMATION('',$,#6937);
#6895=PRODUCT_DEFINITION_FORMATION('',$,#6938);
#6896=PRODUCT_DEFINITION_FORMATION('',$,#6939);
#6897=PRODUCT_DEFINITION_FORMATION('',$,#6940);
#6898=PRODUCT_RELATED_PRODUCT_CATEGORY('PAT-055','PAT-055',(#6921));
#6899=PRODUCT_RELATED_PRODUCT_CATEGORY(
'Extrusion jambs and fixed hinge leaves',
'Extrusion jambs and fixed hinge leaves',(#6922));
#6900=PRODUCT_RELATED_PRODUCT_CATEGORY('Latch strike plate',
'Latch strike plate',(#6923));
#6901=PRODUCT_RELATED_PRODUCT_CATEGORY(
'Slotted Extrusion - 20 x 20 x 300 mm',
'Slotted Extrusion - 20 x 20 x 300 mm',(#6924));
#6902=PRODUCT_RELATED_PRODUCT_CATEGORY('Fixed hinge leaf',
'Fixed hinge leaf',(#6925));
#6903=PRODUCT_RELATED_PRODUCT_CATEGORY('Clevis Pin - 6x30',
'Clevis Pin - 6x30',(#6926));
#6904=PRODUCT_RELATED_PRODUCT_CATEGORY('Flat Washer - M6',
'Flat Washer - M6',(#6927));
#6905=PRODUCT_RELATED_PRODUCT_CATEGORY('Split Pin - 1.6x16',
'Split Pin - 1.6x16',(#6928));
#6906=PRODUCT_RELATED_PRODUCT_CATEGORY(
'Slot Nut - M5 for 20 mm Extrusion','Slot Nut - M5 for 20 mm Extrusion',
(#6929));
#6907=PRODUCT_RELATED_PRODUCT_CATEGORY('M5x14 Cap Screw',
'M5x14 Cap Screw',(#6930));
#6908=PRODUCT_RELATED_PRODUCT_CATEGORY('Panel and moving hinge leaves',
'Panel and moving hinge leaves',(#6931));
#6909=PRODUCT_RELATED_PRODUCT_CATEGORY('Door panel','Door panel',(#6932));
#6910=PRODUCT_RELATED_PRODUCT_CATEGORY('Moving hinge leaf',
'Moving hinge leaf',(#6933));
#6911=PRODUCT_RELATED_PRODUCT_CATEGORY('Cap Screw - M4x16',
'Cap Screw - M4x16',(#6934));
#6912=PRODUCT_RELATED_PRODUCT_CATEGORY('Hex Nut - M4','Hex Nut - M4',(#6935));
#6913=PRODUCT_RELATED_PRODUCT_CATEGORY('Flat Washer - M5',
'Flat Washer - M5',(#6936));
#6914=PRODUCT_RELATED_PRODUCT_CATEGORY('Cap Screw - M5x20',
'Cap Screw - M5x20',(#6937));
#6915=PRODUCT_RELATED_PRODUCT_CATEGORY('Hex Nut - M5','Hex Nut - M5',(#6938));
#6916=PRODUCT_RELATED_PRODUCT_CATEGORY('Turn-button latch',
'Turn-button latch',(#6939));
#6917=PRODUCT_RELATED_PRODUCT_CATEGORY('Turn-button latch (1)',
'Turn-button latch (1)',(#6940));
#6918=APPLICATION_PROTOCOL_DEFINITION('international standard',
'automotive_design',2009,#6919);
#6919=APPLICATION_CONTEXT(
'Core Data for Automotive Mechanical Design Process');
#6920=PRODUCT_CONTEXT('part definition',#6919,'mechanical');
#6921=PRODUCT('PAT-055','PAT-055',
'PAT-055',(#6920));
#6922=PRODUCT('Extrusion jambs and fixed hinge leaves',
'Extrusion jambs and fixed hinge leaves',
'Extrusion jambs and fixed hinge leaves',(#6920));
#6923=PRODUCT('Latch strike plate','Latch strike plate',
'Latch strike plate',(#6920));
#6924=PRODUCT('Slotted Extrusion - 20 x 20 x 300 mm',
'Slotted Extrusion - 20 x 20 x 300 mm',
'Slotted Extrusion - 20 x 20 x 300 mm',(#6920));
#6925=PRODUCT('Fixed hinge leaf','Fixed hinge leaf','Fixed hinge leaf',
(#6920));
#6926=PRODUCT('Clevis Pin - 6x30','Clevis Pin - 6x30',
'Clevis Pin - 6x30',(#6920));
#6927=PRODUCT('Flat Washer - M6','Flat Washer - M6','Flat Washer - M6',
(#6920));
#6928=PRODUCT('Split Pin - 1.6x16','Split Pin - 1.6x16',
'Split Pin - 1.6x16',(#6920));
#6929=PRODUCT('Slot Nut - M5 for 20 mm Extrusion',
'Slot Nut - M5 for 20 mm Extrusion','Slot Nut - M5 for 20 mm Extrusion',
(#6920));
#6930=PRODUCT('M5x14 Cap Screw','M5x14 Cap Screw','M5x14 Cap Screw',(#6920));
#6931=PRODUCT('Panel and moving hinge leaves',
'Panel and moving hinge leaves','Panel and moving hinge leaves',(#6920));
#6932=PRODUCT('Door panel','Door panel','Door panel',(#6920));
#6933=PRODUCT('Moving hinge leaf','Moving hinge leaf',
'Moving hinge leaf',(#6920));
#6934=PRODUCT('Cap Screw - M4x16','Cap Screw - M4x16',
'Cap Screw - M4x16',(#6920));
#6935=PRODUCT('Hex Nut - M4','Hex Nut - M4','Hex Nut - M4',(#6920));
#6936=PRODUCT('Flat Washer - M5','Flat Washer - M5','Flat Washer - M5',
(#6920));
#6937=PRODUCT('Cap Screw - M5x20','Cap Screw - M5x20',
'Cap Screw - M5x20',(#6920));
#6938=PRODUCT('Hex Nut - M5','Hex Nut - M5','Hex Nut - M5',(#6920));
#6939=PRODUCT('Turn-button latch','Turn-button latch',
'Turn-button latch',(#6920));
#6940=PRODUCT('Turn-button latch (1)','Turn-button latch (1)',
'Turn-button latch (1)',(#6920));
#6941=PRESENTATION_STYLE_ASSIGNMENT((#6946));
#6942=PRESENTATION_STYLE_ASSIGNMENT((#6947));
#6943=PRESENTATION_STYLE_ASSIGNMENT((#6948));
#6944=PRESENTATION_STYLE_ASSIGNMENT((#6949));
#6945=PRESENTATION_STYLE_ASSIGNMENT((#6950));
#6946=SURFACE_STYLE_USAGE(.BOTH.,#6951);
#6947=SURFACE_STYLE_USAGE(.BOTH.,#6952);
#6948=SURFACE_STYLE_USAGE(.BOTH.,#6953);
#6949=SURFACE_STYLE_USAGE(.BOTH.,#6954);
#6950=SURFACE_STYLE_USAGE(.BOTH.,#6955);
#6951=SURFACE_SIDE_STYLE('',(#6956));
#6952=SURFACE_SIDE_STYLE('',(#6957));
#6953=SURFACE_SIDE_STYLE('',(#6958));
#6954=SURFACE_SIDE_STYLE('',(#6959));
#6955=SURFACE_SIDE_STYLE('',(#6960));
#6956=SURFACE_STYLE_FILL_AREA(#6961);
#6957=SURFACE_STYLE_FILL_AREA(#6962);
#6958=SURFACE_STYLE_FILL_AREA(#6963);
#6959=SURFACE_STYLE_FILL_AREA(#6964);
#6960=SURFACE_STYLE_FILL_AREA(#6965);
#6961=FILL_AREA_STYLE('Steel - Satin',(#6966));
#6962=FILL_AREA_STYLE('CAD Library Painted - Engineering blue',(#6967));
#6963=FILL_AREA_STYLE('CAD Library Painted - Steel gray',(#6968));
#6964=FILL_AREA_STYLE('CAD Library Painted - Graphite',(#6969));
#6965=FILL_AREA_STYLE('CAD Library Painted - Light blue',(#6970));
#6966=FILL_AREA_STYLE_COLOUR('Steel - Satin',#6971);
#6967=FILL_AREA_STYLE_COLOUR('CAD Library Painted - Engineering blue',#6972);
#6968=FILL_AREA_STYLE_COLOUR('CAD Library Painted - Steel gray',#6973);
#6969=FILL_AREA_STYLE_COLOUR('CAD Library Painted - Graphite',#6974);
#6970=FILL_AREA_STYLE_COLOUR('CAD Library Painted - Light blue',#6975);
#6971=COLOUR_RGB('Steel - Satin',0.627450980392157,0.627450980392157,0.627450980392157);
#6972=COLOUR_RGB('CAD Library Painted - Engineering blue',0.12156862745098,
0.356862745098039,0.6);
#6973=COLOUR_RGB('CAD Library Painted - Steel gray',0.592156862745098,0.631372549019608,
0.67843137254902);
#6974=COLOUR_RGB('CAD Library Painted - Graphite',0.0980392156862745,0.109803921568627,
0.125490196078431);
#6975=COLOUR_RGB('CAD Library Painted - Light blue',0.286274509803922,0.552941176470588,
0.780392156862745);
#6976=COLOUR_RGB('Dark Blue',0.08,0.2,0.34);
#6977=FILL_AREA_STYLE_COLOUR('',#6976);
#6978=FILL_AREA_STYLE('',(#6977));
#6979=SURFACE_STYLE_FILL_AREA(#6978);
#6980=SURFACE_SIDE_STYLE('',(#6979));
#6981=SURFACE_STYLE_USAGE(.BOTH.,#6980);
#6982=PRESENTATION_STYLE_ASSIGNMENT((#6981));
#6983=COLOUR_RGB('Light Blue',0.38,0.62,0.78);
#6984=FILL_AREA_STYLE_COLOUR('',#6983);
#6985=FILL_AREA_STYLE('',(#6984));
#6986=SURFACE_STYLE_FILL_AREA(#6985);
#6987=SURFACE_SIDE_STYLE('',(#6986));
#6988=SURFACE_STYLE_USAGE(.BOTH.,#6987);
#6989=PRESENTATION_STYLE_ASSIGNMENT((#6988));
#6990=COLOUR_RGB('Sky Blue',0.24,0.69,0.87);
#6991=FILL_AREA_STYLE_COLOUR('',#6990);
#6992=FILL_AREA_STYLE('',(#6991));
#6993=SURFACE_STYLE_FILL_AREA(#6992);
#6994=SURFACE_SIDE_STYLE('',(#6993));
#6995=SURFACE_STYLE_USAGE(.BOTH.,#6994);
#6996=PRESENTATION_STYLE_ASSIGNMENT((#6995));
#6997=COLOUR_RGB('Grey',0.48,0.52,0.57);
#6998=FILL_AREA_STYLE_COLOUR('',#6997);
#6999=FILL_AREA_STYLE('',(#6998));
#7000=SURFACE_STYLE_FILL_AREA(#6999);
#7001=SURFACE_SIDE_STYLE('',(#7000));
#7002=SURFACE_STYLE_USAGE(.BOTH.,#7001);
#7003=PRESENTATION_STYLE_ASSIGNMENT((#7002));
#7004=COLOUR_RGB('Black',0.12,0.14,0.17);
#7005=FILL_AREA_STYLE_COLOUR('',#7004);
#7006=FILL_AREA_STYLE('',(#7005));
#7007=SURFACE_STYLE_FILL_AREA(#7006);
#7008=SURFACE_SIDE_STYLE('',(#7007));
#7009=SURFACE_STYLE_USAGE(.BOTH.,#7008);
#7010=PRESENTATION_STYLE_ASSIGNMENT((#7009));
#7011=COLOUR_RGB('Off White',0.89,0.88,0.83);
#7012=FILL_AREA_STYLE_COLOUR('',#7011);
#7013=FILL_AREA_STYLE('',(#7012));
#7014=SURFACE_STYLE_FILL_AREA(#7013);
#7015=SURFACE_SIDE_STYLE('',(#7014));
#7016=SURFACE_STYLE_USAGE(.BOTH.,#7015);
#7017=PRESENTATION_STYLE_ASSIGNMENT((#7016));
ENDSEC;
END-ISO-10303-21;
